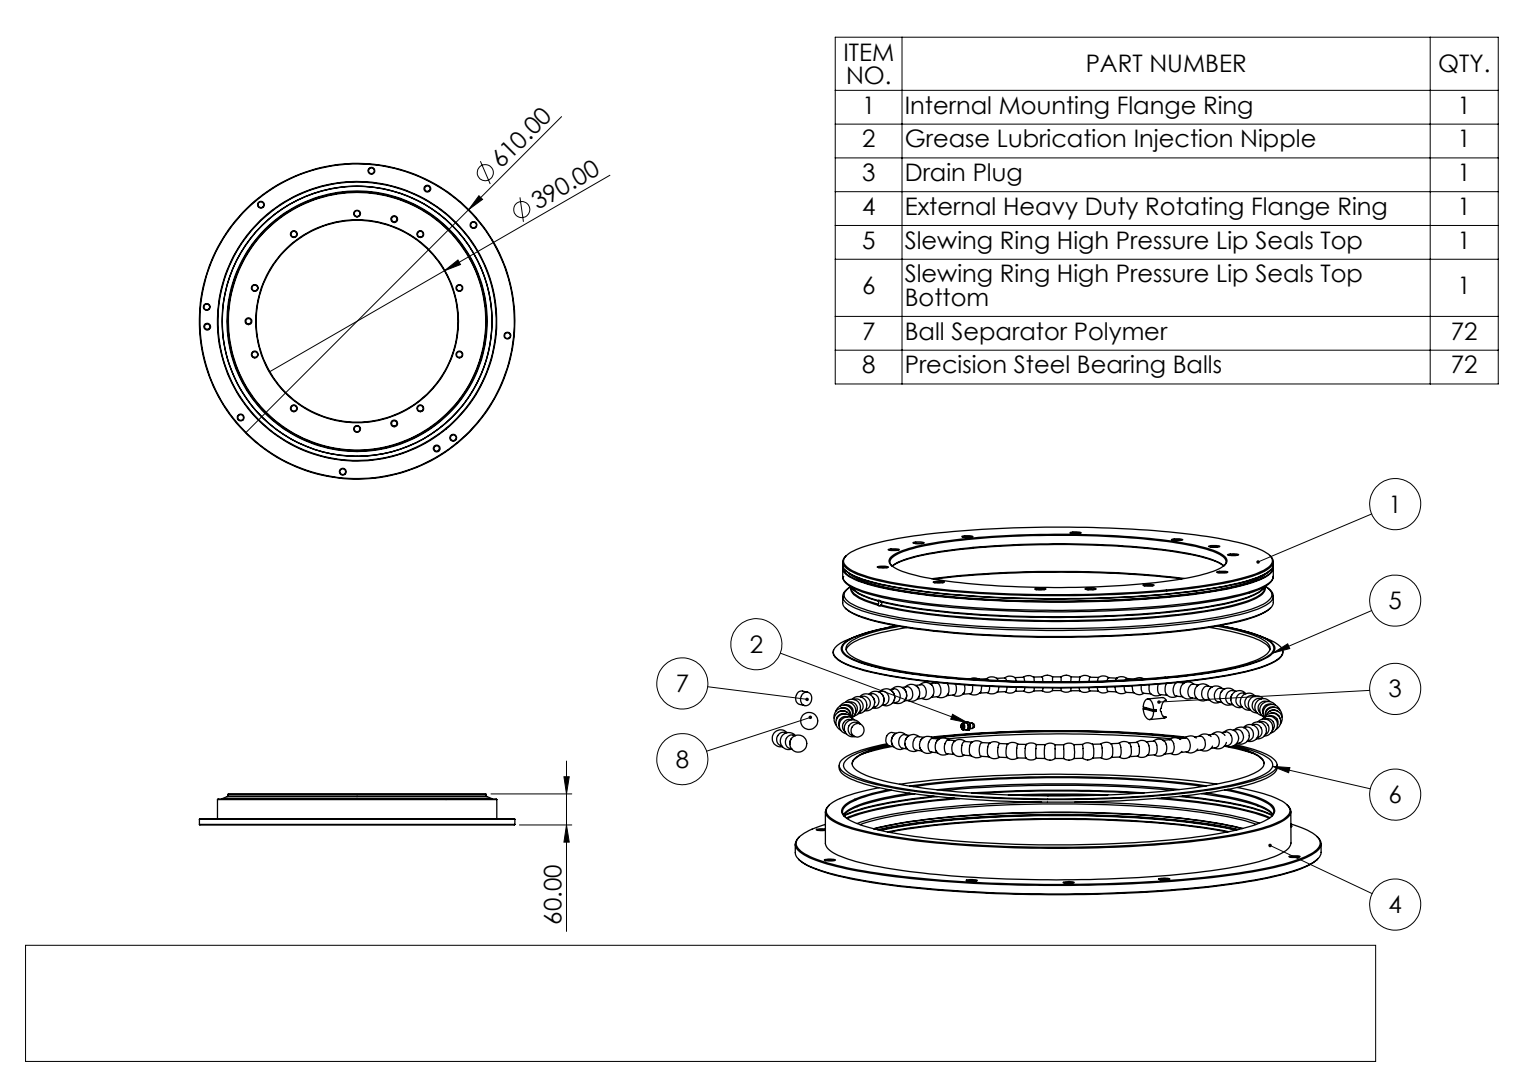
ISO-10303-21;
HEADER;
FILE_DESCRIPTION (('STEP AP214'),
    '1' );
FILE_NAME ('MAS-489',
    '2026-10-09T12:49:55',
    ( '' ),
    ( '' ),
    'SwSTEP 2.0',
    'SolidWorks 2026',
    '' );
FILE_SCHEMA (( 'AUTOMOTIVE_DESIGN' ));
ENDSEC;

DATA;
#1 = CARTESIAN_POINT ( 'NONE',  ( -244.7604950974910878, 8.603785962528602838, 8.365103762022689793 ) ) ;
#2 = VECTOR ( 'NONE', #2010, 1000.000000000000000 ) ;
#3 = DIRECTION ( 'NONE',  ( 0.6378047977532573798, 0.5538822189107470706, -0.5351817705578485462 ) ) ;
#4 = CARTESIAN_POINT ( 'NONE',  ( 227.3999999999999773, -2.172755033604258923, 3.940702420120982374 ) ) ;
#5 = TOROIDAL_SURFACE ( 'NONE', #5776, 250.0000000000000000, 10.00000000000000000 ) ;
#6 = ITEM_DEFINED_TRANSFORMATION ( 'NONE', 'NONE', #11295,  #805 ) ;
#7 = CARTESIAN_POINT ( 'NONE',  ( 222.8706404512946904, 0.000000000000000000, 0.000000000000000000 ) ) ;
#8 = EDGE_LOOP ( 'NONE', ( #2627, #6093, #4363, #303 ) ) ;
#9 = ORIENTED_EDGE ( 'NONE', *, *, #8914, .T. ) ;
#10 = CONICAL_SURFACE ( 'NONE', #3613, 1.750000000000000000, 0.4188790204786330129 ) ;
#11 = CARTESIAN_POINT ( 'NONE',  ( -34.18476129408180242, 19.96883745937779864, 259.4723857443443080 ) ) ;
#12 = DIRECTION ( 'NONE',  ( 0.000000000000000000, -1.000000000000000000, 0.000000000000000000 ) ) ;
#13 = ADVANCED_FACE ( 'NONE', ( #7160 ), #9859, .F. ) ;
#14 = EDGE_CURVE ( 'NONE', #2438, #5570, #3411, .T. ) ;
#15 = DIRECTION ( 'NONE',  ( 0.6368676505102708330, 0.000000000000000000, 0.7709731485165535192 ) ) ;
#16 = AXIS2_PLACEMENT_3D ( 'NONE', #743, #4857, #3859 ) ;
#17 = CARTESIAN_POINT ( 'NONE',  ( 17.06760680892275062, 20.79694577654979071, 260.7745447056980197 ) ) ;
#18 = CYLINDRICAL_SURFACE ( 'NONE', #6462, 5.500000000000005329 ) ;
#19 = DIRECTION ( 'NONE',  ( 0.5735764363510555963, 0.000000000000000000, -0.8191520442889851372 ) ) ;
#20 = CARTESIAN_POINT ( 'NONE',  ( -243.1949234122827193, -7.480730365350286348, 9.061063672199042074 ) ) ;
#21 = CONTEXT_DEPENDENT_SHAPE_REPRESENTATION ( #3190, #1979 ) ;
#22 = ORIENTED_EDGE ( 'NONE', *, *, #3438, .F. ) ;
#23 = CARTESIAN_POINT ( 'NONE',  ( -230.0000000000000000, 18.00000000000000000, 0.000000000000000000 ) ) ;
#24 = LINE ( 'NONE', #4986, #10827 ) ;
#25 = CARTESIAN_POINT ( 'NONE',  ( 0.000000000000000000, 22.00000000000000000, 0.000000000000000000 ) ) ;
#26 = EDGE_LOOP ( 'NONE', ( #5879, #12768 ) ) ;
#27 = ORIENTED_EDGE ( 'NONE', *, *, #7436, .F. ) ;
#28 = DIRECTION ( 'NONE',  ( 0.000000000000000000, 1.000000000000000000, 0.000000000000000000 ) ) ;
#29 = PLANE ( 'NONE',  #10608 ) ;
#30 = CARTESIAN_POINT ( 'NONE',  ( -247.8175805190998062, 19.96883746075563693, 84.14846197946620521 ) ) ;
#31 = VECTOR ( 'NONE', #3967, 1000.000000000000000 ) ;
#32 = STYLED_ITEM ( 'NONE', ( #1106 ), #1548 ) ;
#33 = CARTESIAN_POINT ( 'NONE',  ( 122.2593324768346008, 18.00000000000000000, 161.7755348299889988 ) ) ;
#34 = AXIS2_PLACEMENT_3D ( 'NONE', #11717, #7639, #3504 ) ;
#35 = DIRECTION ( 'NONE',  ( 0.9659258262890680902, 0.000000000000000000, 0.2588190451025213501 ) ) ;
#36 = CARTESIAN_POINT ( 'NONE',  ( -244.7823818444411188, 8.610125652527095497, 7.996289171610727387 ) ) ;
#37 = EDGE_LOOP ( 'NONE', ( #12294, #12083 ) ) ;
#38 = CARTESIAN_POINT ( 'NONE',  ( 206.9952515782970295, 20.79694577634646535, 158.8368823490022237 ) ) ;
#39 = EDGE_CURVE ( 'NONE', #10768, #6987, #12629, .T. ) ;
#41 = ORIENTED_EDGE ( 'NONE', *, *, #3287, .F. ) ;
#40 = AXIS2_PLACEMENT_3D ( 'NONE', #6246, #10297, #1175 ) ;
#42 = EDGE_CURVE ( 'NONE', #9318, #6702, #6889, .T. ) ;
#43 = CARTESIAN_POINT ( 'NONE',  ( 6.735557395310442023E-16, 19.00000000000000000, 213.5000000000000000 ) ) ;
#44 = ORIENTED_EDGE ( 'NONE', *, *, #3957, .F. ) ;
#45 = CARTESIAN_POINT ( 'NONE',  ( -248.8440518482232733, 9.943161799075943108, -6.718187330775476696 ) ) ;
#46 =( REPRESENTATION_RELATIONSHIP ('NONE','NONE', #12019, #182 ) REPRESENTATION_RELATIONSHIP_WITH_TRANSFORMATION ( #319 )SHAPE_REPRESENTATION_RELATIONSHIP( ) );
#47 = DIRECTION ( 'NONE',  ( -0.000000000000000000, 1.000000000000000000, 0.000000000000000000 ) ) ;
#48 = SURFACE_SIDE_STYLE ('',( #1037 ) ) ;
#49 = CYLINDRICAL_SURFACE ( 'NONE', #12751, 249.7999999999999829 ) ;
#50 = CARTESIAN_POINT ( 'NONE',  ( 6.735557395310442023E-16, 19.00000000000000000, -202.4999999999999716 ) ) ;
#51 = CARTESIAN_POINT ( 'NONE',  ( 6.345753394971347358E-13, 20.08915143297736350, -260.5542428351130866 ) ) ;
#52 = DIRECTION ( 'NONE',  ( 0.000000000000000000, -1.000000000000000000, 0.000000000000000000 ) ) ;
#53 = CARTESIAN_POINT ( 'NONE',  ( -137.7829567244536122, 20.79694577634646890, 221.5672498511017920 ) ) ;
#54 = ITEM_DEFINED_TRANSFORMATION ( 'NONE', 'NONE', #1459,  #805 ) ;
#55 = ORIENTED_EDGE ( 'NONE', *, *, #3049, .F. ) ;
#56 = CARTESIAN_POINT ( 'NONE',  ( 220.3999999999999773, 2.249562960690858038, -0.04434507737934524629 ) ) ;
#57 = CIRCLE ( 'NONE', #1754, 6.500000000000005329 ) ;
#58 = VERTEX_POINT ( 'NONE', #5076 ) ;
#59 = EDGE_CURVE ( 'NONE', #2857, #11921, #819, .T. ) ;
#60 = CIRCLE ( 'NONE', #11338, 5.499999999999986677 ) ;
#61 = CARTESIAN_POINT ( 'NONE',  ( -249.1369139485392168, 10.36343465138863529, -5.538914405136962316 ) ) ;
#62 = CARTESIAN_POINT ( 'NONE',  ( -246.4289107134841004, -9.384359667671809291, -7.479355995036127247 ) ) ;
#63 =( REPRESENTATION_RELATIONSHIP ('NONE','NONE', #12019, #182 ) REPRESENTATION_RELATIONSHIP_WITH_TRANSFORMATION ( #9414 )SHAPE_REPRESENTATION_RELATIONSHIP( ) );
#64 = DIRECTION ( 'NONE',  ( 0.6368676505102698338, 0.000000000000000000, 0.7709731485165541853 ) ) ;
#65 = ORIENTED_EDGE ( 'NONE', *, *, #5983, .T. ) ;
#66 = ADVANCED_FACE ( 'NONE', ( #7091 ), #10088, .F. ) ;
#67 = CARTESIAN_POINT ( 'NONE',  ( 84.02568524182660781, 20.79694577630801078, -247.4557548099990072 ) ) ;
#68 = DIRECTION ( 'NONE',  ( 8.659560562354926695E-17, 0.7071067811865480168, -0.7071067811865470176 ) ) ;
#69 = CARTESIAN_POINT ( 'NONE',  ( -239.9450917581429792, -2.156506209390995021, 11.80463811257499884 ) ) ;
#70 = AXIS2_PLACEMENT_3D ( 'NONE', #7490, #8365, #9292 ) ;
#71 = CARTESIAN_POINT ( 'NONE',  ( -245.4148443366356389, -8.946846751066603431, -7.616852152915439156 ) ) ;
#72 = DIRECTION ( 'NONE',  ( 0.7545873610930060593, 0.5538822189107471816, -0.3518698652246315395 ) ) ;
#73 = CARTESIAN_POINT ( 'NONE',  ( -229.7583704989254443, -5.204493534573133573, 10.54155285988093382 ) ) ;
#74 = PRODUCT_DEFINITION_SHAPE ( 'NONE', 'NONE',  #13116 ) ;
#75 = CIRCLE ( 'NONE', #5391, 251.1999999999999886 ) ;
#76 = CARTESIAN_POINT ( 'NONE',  ( 0.000000000000000000, -23.50000000000000000, 0.000000000000000000 ) ) ;
#77 = AXIS2_PLACEMENT_3D ( 'NONE', #6499, #10557, #9543 ) ;
#78 = ORIENTED_EDGE ( 'NONE', *, *, #7931, .F. ) ;
#79 = ORIENTED_EDGE ( 'NONE', *, *, #10538, .F. ) ;
#80 = CARTESIAN_POINT ( 'NONE',  ( 247.2466869557899827, 20.08915143289970473, -83.95474316006121285 ) ) ;
#81 = CARTESIAN_POINT ( 'NONE',  ( 11.00000000000000000, 0.000000000000000000, 259.9000000000000341 ) ) ;
#82 = FACE_OUTER_BOUND ( 'NONE', #8092, .T. ) ;
#83 = DIRECTION ( 'NONE',  ( -0.000000000000000000, -1.000000000000000000, 0.000000000000000000 ) ) ;
#84 = CIRCLE ( 'NONE', #11996, 6.500000000000005329 ) ;
#85 = CARTESIAN_POINT ( 'NONE',  ( -1.010328782420808020E-12, 20.79694577634649022, 260.7745447061710138 ) ) ;
#86 = CARTESIAN_POINT ( 'NONE',  ( -182.4625818711933221, -29.00000000000000000, -220.8838070499919297 ) ) ;
#87 = DIRECTION ( 'NONE',  ( 0.9659258262890654256, 0.000000000000000000, 0.2588190451025314531 ) ) ;
#88 = CONICAL_SURFACE ( 'NONE', #12605, 5.500000000000005329, 0.7853981633974461696 ) ;
#89 = CARTESIAN_POINT ( 'NONE',  ( -243.1551830321760690, -7.446108171798711872, 9.089443071778552152 ) ) ;
#90 = VERTEX_POINT ( 'NONE', #9222 ) ;
#91 = FACE_BOUND ( 'NONE', #3077, .T. ) ;
#92 = EDGE_CURVE ( 'NONE', #10082, #1949, #2942, .T. ) ;
#93 = DIRECTION ( 'NONE',  ( 0.000000000000000000, 1.000000000000000000, 0.000000000000000000 ) ) ;
#94 = ORIENTED_EDGE ( 'NONE', *, *, #12232, .T. ) ;
#95 = ORIENTED_EDGE ( 'NONE', *, *, #11589, .F. ) ;
#96 = CONICAL_SURFACE ( 'NONE', #12225, 250.1999999999999602, 0.7853981633975041232 ) ;
#97 = DIRECTION ( 'NONE',  ( 0.000000000000000000, 0.000000000000000000, -1.000000000000000000 ) ) ;
#98 = FACE_BOUND ( 'NONE', #10727, .T. ) ;
#99 = CARTESIAN_POINT ( 'NONE',  ( 34.18476129334108293, 19.96883746037050855, -259.4723857425807978 ) ) ;
#100 = CARTESIAN_POINT ( 'NONE',  ( -294.8238222686197787, -18.00000000000000000, -32.70078231947154279 ) ) ;
#101 = CARTESIAN_POINT ( 'NONE',  ( 0.000000000000000000, 0.000000000000000000, 0.000000000000000000 ) ) ;
#102 = CARTESIAN_POINT ( 'NONE',  ( -243.6022064859786269, 7.815160994106106429, 8.774769236968495534 ) ) ;
#103 = CONICAL_SURFACE ( 'NONE', #1806, 5.500000000000005329, 0.7853981633974461696 ) ;
#104 = AXIS2_PLACEMENT_3D ( 'NONE', #9793, #603, #2593 ) ;
#105 = EDGE_LOOP ( 'NONE', ( #5377, #568, #8957, #6732 ) ) ;
#106 = FACE_OUTER_BOUND ( 'NONE', #3222, .T. ) ;
#107 = EDGE_CURVE ( 'NONE', #6490, #4415, #2518, .T. ) ;
#108 = EDGE_LOOP ( 'NONE', ( #11966, #7349 ) ) ;
#109 = CARTESIAN_POINT ( 'NONE',  ( 234.3487510399341716, 2.474519256759935448, -0.04877958511727960994 ) ) ;
#110 = ORIENTED_EDGE ( 'NONE', *, *, #7597, .T. ) ;
#111 = ORIENTED_EDGE ( 'NONE', *, *, #3767, .F. ) ;
#112 = CIRCLE ( 'NONE', #2851, 5.500000000000007994 ) ;
#113 = CARTESIAN_POINT ( 'NONE',  ( 229.2637990951503753, -30.00000000000000000, -180.9540284836414514 ) ) ;
#114 = FILL_AREA_STYLE_COLOUR ( '', #3598 ) ;
#115 = PRODUCT ( 'MAS-489', 'MAS-489', '', ( #1262 ) ) ;
#116 = CARTESIAN_POINT ( 'NONE',  ( 239.1963018252363042, 1.024882057239583366, 3.346595946712579206 ) ) ;
#117 = EDGE_CURVE ( 'NONE', #171, #5643, #5501, .T. ) ;
#118 = DIRECTION ( 'NONE',  ( -0.000000000000000000, -1.000000000000000000, 0.000000000000000000 ) ) ;
#119 = EDGE_CURVE ( 'NONE', #4577, #1020, #8907, .T. ) ;
#120 = CARTESIAN_POINT ( 'NONE',  ( -238.7109915777814138, -2.671037648644427152E-08, -11.74999999995326050 ) ) ;
#121 = DIRECTION ( 'NONE',  ( 0.000000000000000000, 1.000000000000000000, 0.000000000000000000 ) ) ;
#122 = ITEM_DEFINED_TRANSFORMATION ( 'NONE', 'NONE', #4000,  #805 ) ;
#123 = ORIENTED_EDGE ( 'NONE', *, *, #7186, .T. ) ;
#124 = DIRECTION ( 'NONE',  ( -0.6368676505102700558, 0.000000000000000000, -0.7709731485165541853 ) ) ;
#125 = AXIS2_PLACEMENT_3D ( 'NONE', #10456, #7067, #12062 ) ;
#126 = ORIENTED_EDGE ( 'NONE', *, *, #7506, .T. ) ;
#127 = CIRCLE ( 'NONE', #974, 239.8169934640564804 ) ;
#128 = FACE_OUTER_BOUND ( 'NONE', #4868, .T. ) ;
#129 = CARTESIAN_POINT ( 'NONE',  ( -248.5349130519067558, -9.924317173753149035, -6.749248572539269020 ) ) ;
#130 = CARTESIAN_POINT ( 'NONE',  ( 67.47543992452018813, 20.08915143297736705, -251.8100110699623713 ) ) ;
#131 = EDGE_LOOP ( 'NONE', ( #6897, #5787, #9258, #12917 ) ) ;
#132 = CARTESIAN_POINT ( 'NONE',  ( 252.4341100445949735, 20.79694577582237613, 67.61424742981928659 ) ) ;
#133 = CARTESIAN_POINT ( 'NONE',  ( -244.3545189613893172, 8.356296381722604139, -8.612604416346371750 ) ) ;
#134 = DIRECTION ( 'NONE',  ( 0.000000000000000000, 0.000000000000000000, 1.000000000000000000 ) ) ;
#135 = EDGE_CURVE ( 'NONE', #12433, #12610, #12359, .T. ) ;
#136 = CARTESIAN_POINT ( 'NONE',  ( -243.1925160140377216, -7.478514340598183097, -9.062807757124144103 ) ) ;
#137 = ADVANCED_FACE ( 'NONE', ( #98, #7027 ), #29, .F. ) ;
#138 = CARTESIAN_POINT ( 'NONE',  ( 39.32730324096118579, -138.4705547276867321, 14.31396777367110928 ) ) ;
#139 = CARTESIAN_POINT ( 'NONE',  ( 240.4181131690920097, 2.891045149275324633, 1.982248008065000233 ) ) ;
#140 = EDGE_CURVE ( 'NONE', #10237, #12935, #11247, .T. ) ;
#141 = ITEM_DEFINED_TRANSFORMATION ( 'NONE', 'NONE', #2560,  #805 ) ;
#142 = CARTESIAN_POINT ( 'NONE',  ( -27.68945685411286561, -30.00000000000000000, 290.6841825403027997 ) ) ;
#143 = ORIENTED_EDGE ( 'NONE', *, *, #1183, .T. ) ;
#144 = ORIENTED_EDGE ( 'NONE', *, *, #3305, .F. ) ;
#145 = CARTESIAN_POINT ( 'NONE',  ( -172.1812796679919870, 20.08915143287683591, 196.2980642839890209 ) ) ;
#146 = FACE_OUTER_BOUND ( 'NONE', #6350, .T. ) ;
#147 = CARTESIAN_POINT ( 'NONE',  ( 239.5387464286556565, -1.581210110862248941, -3.124650852508605858 ) ) ;
#148 = CARTESIAN_POINT ( 'NONE',  ( -185.9653539489998195, -30.00000000000000000, -225.1241593668329699 ) ) ;
#149 = DIRECTION ( 'NONE',  ( 0.000000000000000000, 1.000000000000000000, 0.000000000000000000 ) ) ;
#150 = CARTESIAN_POINT ( 'NONE',  ( 0.000000000000000000, -9.830508068699650437, 0.000000000000000000 ) ) ;
#151 = DIRECTION ( 'NONE',  ( 0.3420201433256790380, 0.000000000000000000, -0.9396926207859046531 ) ) ;
#152 = CARTESIAN_POINT ( 'NONE',  ( -246.6649006625763718, -9.461692665201230312, 6.966985664009688328 ) ) ;
#153 =( REPRESENTATION_RELATIONSHIP ('NONE','NONE', #12019, #5191 ) REPRESENTATION_RELATIONSHIP_WITH_TRANSFORMATION ( #11550 )SHAPE_REPRESENTATION_RELATIONSHIP( ) );
#154 = EDGE_LOOP ( 'NONE', ( #1351, #3008, #4241, #9314 ) ) ;
#155 = CARTESIAN_POINT ( 'NONE',  ( 240.6084075703383292, -3.437342788167941698, 0.6677429272691086659 ) ) ;
#156 = CARTESIAN_POINT ( 'NONE',  ( 229.9948761773756587, -3.146545554286515056, -1.549783278019676303 ) ) ;
#157 = VERTEX_POINT ( 'NONE', #8121 ) ;
#158 = VERTEX_POINT ( 'NONE', #1956 ) ;
#159 = CARTESIAN_POINT ( 'NONE',  ( 122.2593324768334071, 18.00000000000000000, -168.2755348299895104 ) ) ;
#160 = DIRECTION ( 'NONE',  ( 0.000000000000000000, 1.000000000000000000, 0.000000000000000000 ) ) ;
#161 = EDGE_CURVE ( 'NONE', #12208, #12419, #5216, .T. ) ;
#162 = CARTESIAN_POINT ( 'NONE',  ( -172.5787240293117293, 19.96883745935916821, -196.7513681803530403 ) ) ;
#163 = AXIS2_PLACEMENT_3D ( 'NONE', #4831, #2895, #11790 ) ;
#164 = LINE ( 'NONE', #1161, #5159 ) ;
#165 = SHAPE_REPRESENTATION_RELATIONSHIP ( 'NONE' , 'NONE' ,  #182, #11264 ) ;
#166 = CARTESIAN_POINT ( 'NONE',  ( -242.4885533041308179, 6.811171349317773682, 9.574815119040657407 ) ) ;
#167 = VERTEX_POINT ( 'NONE', #4213 ) ;
#168 = CARTESIAN_POINT ( 'NONE',  ( 158.8368823490023374, 20.79694577634646535, 206.9952515782968874 ) ) ;
#169 = VERTEX_POINT ( 'NONE', #4404 ) ;
#170 = CARTESIAN_POINT ( 'NONE',  ( 226.1499999999999773, 0.000000000000000000, 0.000000000000000000 ) ) ;
#171 = VERTEX_POINT ( 'NONE', #8621 ) ;
#172 = ORIENTED_EDGE ( 'NONE', *, *, #9218, .F. ) ;
#173 =( REPRESENTATION_RELATIONSHIP ('NONE','NONE', #12019, #5191 ) REPRESENTATION_RELATIONSHIP_WITH_TRANSFORMATION ( #7916 )SHAPE_REPRESENTATION_RELATIONSHIP( ) );
#174 = DIRECTION ( 'NONE',  ( 0.000000000000000000, -1.000000000000000000, 0.000000000000000000 ) ) ;
#175 = FACE_OUTER_BOUND ( 'NONE', #11352, .T. ) ;
#176 = ADVANCED_FACE ( 'NONE', ( #6424 ), #11036, .F. ) ;
#177 = ADVANCED_FACE ( 'NONE', ( #3475, #8488, #10550, #7486, #12547, #4470, #3403, #10415, #12679, #11557, #2351, #9424, #1290 ), #8427, .F. ) ;
#178 = DIRECTION ( 'NONE',  ( 0.000000000000000000, 0.000000000000000000, 1.000000000000000000 ) ) ;
#179 = CARTESIAN_POINT ( 'NONE',  ( -206.8203823583188807, 20.08915143297736705, -158.7026972336036295 ) ) ;
#180 = LINE ( 'NONE', #8188, #691 ) ;
#181 = AXIS2_PLACEMENT_3D ( 'NONE', #12668, #7601, #11676 ) ;
#182 = SHAPE_REPRESENTATION ( 'Precision Steel Bearing Balls', ( #805 ), #1451 ) ;
#183 = ORIENTED_EDGE ( 'NONE', *, *, #8273, .T. ) ;
#184 = EDGE_LOOP ( 'NONE', ( #4999, #5010, #6703, #1968 ) ) ;
#185 = DIRECTION ( 'NONE',  ( 0.000000000000000000, 0.000000000000000000, 1.000000000000000000 ) ) ;
#186 = DIRECTION ( 'NONE',  ( 0.000000000000000000, 1.000000000000000000, 0.000000000000000000 ) ) ;
#187 = DIRECTION ( 'NONE',  ( 0.6368676505102709440, 0.000000000000000000, 0.7709731485165532971 ) ) ;
#188 = CIRCLE ( 'NONE', #5900, 6.499999999999999112 ) ;
#189 = EDGE_LOOP ( 'NONE', ( #9728, #4932, #9679, #1428 ) ) ;
#190 = VECTOR ( 'NONE', #5245, 1000.000000000000000 ) ;
#191 = CIRCLE ( 'NONE', #10174, 8.000000000000007105 ) ;
#192 = AXIS2_PLACEMENT_3D ( 'NONE', #6124, #12263, #134 ) ;
#193 = CARTESIAN_POINT ( 'NONE',  ( 252.4341100441809829, 20.79694577595645910, -67.61424743030308093 ) ) ;
#194 = CARTESIAN_POINT ( 'NONE',  ( -244.9313462844523315, 8.700834631118880225, -8.264179333829037688 ) ) ;
#195 = CARTESIAN_POINT ( 'NONE',  ( -159.9811538081800393, -30.00000000000000000, -193.6684549073582389 ) ) ;
#196 = CARTESIAN_POINT ( 'NONE',  ( -246.9758887735252699, -9.561393943077655777, -6.829510937495726353 ) ) ;
#197 = CIRCLE ( 'NONE', #11695, 196.0000000000000000 ) ;
#198 = DIRECTION ( 'NONE',  ( 0.7071067811865561215, 0.000000000000000000, -0.7071067811865389130 ) ) ;
#199 = CARTESIAN_POINT ( 'NONE',  ( 240.6075165363340318, 3.437532598196324063, 0.7648284528981581509 ) ) ;
#200 = EDGE_CURVE ( 'NONE', #7619, #9887, #12317, .T. ) ;
#201 = EDGE_CURVE ( 'NONE', #6448, #6354, #188, .T. ) ;
#202 = CARTESIAN_POINT ( 'NONE',  ( 84.02568524192950861, 20.79694577611522632, 247.4557548104415048 ) ) ;
#203 = CIRCLE ( 'NONE', #9142, 2.000000000000001776 ) ;
#204 = VERTEX_POINT ( 'NONE', #489 ) ;
#205 = CARTESIAN_POINT ( 'NONE',  ( 258.8746690706130380, 20.08915143329827657, -34.10614053547809732 ) ) ;
#206 = DIRECTION ( 'NONE',  ( 0.6368676505102707219, 0.000000000000000000, 0.7709731485165535192 ) ) ;
#207 = CARTESIAN_POINT ( 'NONE',  ( -248.9051445890450225, 10.17462340872661741, 5.878044170807267044 ) ) ;
#208 = DIRECTION ( 'NONE',  ( 0.000000000000000000, 0.7071067811865480168, 0.7071067811865470176 ) ) ;
#209 = DIRECTION ( 'NONE',  ( 8.659560562354913137E-17, -0.7071067811865489050, 0.7071067811865460184 ) ) ;
#210 = CARTESIAN_POINT ( 'NONE',  ( -249.3376476200290028, -9.985526825745921542, 6.655116011123642927 ) ) ;
#211 = DIRECTION ( 'NONE',  ( 0.000000000000000000, 0.000000000000000000, 1.000000000000000000 ) ) ;
#212 = DIRECTION ( 'NONE',  ( 0.9848077530122105738, 0.000000000000000000, -0.1736481776669172861 ) ) ;
#213 = DIRECTION ( 'NONE',  ( 0.000000000000000000, 0.000000000000000000, -1.000000000000000000 ) ) ;
#214 = CONTEXT_DEPENDENT_SHAPE_REPRESENTATION ( #9747, #1764 ) ;
#215 = ORIENTED_EDGE ( 'NONE', *, *, #11212, .T. ) ;
#216 = DIRECTION ( 'NONE',  ( 0.000000000000000000, 0.000000000000000000, 1.000000000000000000 ) ) ;
#217 = AXIS2_PLACEMENT_3D ( 'NONE', #2589, #10592, #3388 ) ;
#218 = EDGE_CURVE ( 'NONE', #9833, #1462, #5421, .T. ) ;
#219 = PRODUCT ( 'Grease Lubrication Injection Nipple', 'Grease Lubrication Injection Nipple', '', ( #6400 ) ) ;
#220 = CYLINDRICAL_SURFACE ( 'NONE', #828, 246.0000000000000000 ) ;
#221 = ORIENTED_EDGE ( 'NONE', *, *, #12738, .T. ) ;
#222 = ORIENTED_EDGE ( 'NONE', *, *, #3793, .T. ) ;
#223 = FACE_OUTER_BOUND ( 'NONE', #154, .T. ) ;
#224 = DIRECTION ( 'NONE',  ( 0.000000000000000000, 0.000000000000000000, 1.000000000000000000 ) ) ;
#225 = CARTESIAN_POINT ( 'NONE',  ( -252.9796497735838443, 20.55460285104794949, 67.76049180365761515 ) ) ;
#226 = LINE ( 'NONE', #5219, #2394 ) ;
#227 = CARTESIAN_POINT ( 'NONE',  ( 0.000000000000000000, 0.000000000000000000, 0.000000000000000000 ) ) ;
#228 = DIRECTION ( 'NONE',  ( 0.000000000000000000, 0.000000000000000000, 1.000000000000000000 ) ) ;
#229 = AXIS2_PLACEMENT_3D ( 'NONE', #9662, #409, #545 ) ;
#230 = ORIENTED_EDGE ( 'NONE', *, *, #4416, .F. ) ;
#231 = DIRECTION ( 'NONE',  ( 1.000000000000000000, 0.000000000000000000, 0.000000000000000000 ) ) ;
#232 = ORIENTED_EDGE ( 'NONE', *, *, #7024, .T. ) ;
#233 = CARTESIAN_POINT ( 'NONE',  ( 135.8846079354933352, -18.00000000000000000, -256.1940150085812888 ) ) ;
#234 = ORIENTED_EDGE ( 'NONE', *, *, #10382, .T. ) ;
#235 = ORIENTED_EDGE ( 'NONE', *, *, #8600, .T. ) ;
#236 = CARTESIAN_POINT ( 'NONE',  ( 222.0845275804282153, 0.000000000000000000, 0.000000000000000000 ) ) ;
#237 = VERTEX_POINT ( 'NONE', #3498 ) ;
#238 = DIRECTION ( 'NONE',  ( 0.000000000000000000, 1.000000000000000000, 0.000000000000000000 ) ) ;
#239 = CARTESIAN_POINT ( 'NONE',  ( -171.9542656377731475, 19.00000000000000000, -208.1627500994694344 ) ) ;
#240 = CARTESIAN_POINT ( 'NONE',  ( 11.00000000000000000, 0.000000000000000000, 250.0000000000000000 ) ) ;
#241 = CARTESIAN_POINT ( 'NONE',  ( -233.0000000000000000, 1.000000000000000000, 11.95826074310140008 ) ) ;
#242 = CARTESIAN_POINT ( 'NONE',  ( -243.4813404522815574, 7.728679802368522367, 9.179736092244874968 ) ) ;
#243 = DIRECTION ( 'NONE',  ( 0.000000000000000000, -0.7071067811865489050, -0.7071067811865460184 ) ) ;
#244 = CONTEXT_DEPENDENT_SHAPE_REPRESENTATION ( #46, #6907 ) ;
#245 = ORIENTED_EDGE ( 'NONE', *, *, #2691, .F. ) ;
#246 = DIRECTION ( 'NONE',  ( 0.9135454576426030870, 0.4066576386751317163, -0.008016341293427224970 ) ) ;
#247 = AXIS2_PLACEMENT_3D ( 'NONE', #6656, #10577, #2507 ) ;
#248 = CARTESIAN_POINT ( 'NONE',  ( -249.2724874750463755, -10.50618518648515476, 5.261424415983393388 ) ) ;
#249 = ORIENTED_EDGE ( 'NONE', *, *, #11663, .F. ) ;
#250 = DIRECTION ( 'NONE',  ( -0.6368676505102706109, 0.000000000000000000, -0.7709731485165535192 ) ) ;
#251 = DIRECTION ( 'NONE',  ( -0.000000000000000000, -1.000000000000000000, 0.000000000000000000 ) ) ;
#252 = EDGE_CURVE ( 'NONE', #8118, #6913, #791, .T. ) ;
#253 = EDGE_CURVE ( 'NONE', #823, #11992, #3550, .T. ) ;
#254 = DIRECTION ( 'NONE',  ( 0.000000000000000000, 0.000000000000000000, 1.000000000000000000 ) ) ;
#255 = ORIENTED_EDGE ( 'NONE', *, *, #1182, .T. ) ;
#256 = CARTESIAN_POINT ( 'NONE',  ( -233.0000000000000000, 0.000000000000000000, 0.000000000000000000 ) ) ;
#257 = CARTESIAN_POINT ( 'NONE',  ( -241.6004288480548610, 5.767183905335713234, -10.52387470031727368 ) ) ;
#258 = CARTESIAN_POINT ( 'NONE',  ( -238.7266973618091299, 0.3758472202226714187, 11.99420542475303009 ) ) ;
#259 = CARTESIAN_POINT ( 'NONE',  ( -229.9627996858143888, 10.99879348686639879, 4.151745503392231029 ) ) ;
#260 = AXIS2_PLACEMENT_3D ( 'NONE', #6805, #2654, #10860 ) ;
#261 = FILL_AREA_STYLE_COLOUR ( '', #9272 ) ;
#262 = APPLICATION_PROTOCOL_DEFINITION ( 'draft international standard', 'automotive_design', 1998, #8164 ) ;
#263 = CARTESIAN_POINT ( 'NONE',  ( -229.6996873213522008, 2.466058644897756835, -11.74980236389214028 ) ) ;
#264 = CONTEXT_DEPENDENT_SHAPE_REPRESENTATION ( #5876, #9605 ) ;
#265 = AXIS2_PLACEMENT_3D ( 'NONE', #9269, #11198, #3992 ) ;
#266 = FACE_OUTER_BOUND ( 'NONE', #2939, .T. ) ;
#267 = ORIENTED_EDGE ( 'NONE', *, *, #6171, .T. ) ;
#268 = CONICAL_SURFACE ( 'NONE', #4306, 251.1999999999999886, 0.7853981633974207455 ) ;
#269 = CARTESIAN_POINT ( 'NONE',  ( 172.1812796672219861, 20.08915143311016749, 196.2980642831085163 ) ) ;
#270 = PLANE ( 'NONE',  #8814 ) ;
#271 = CARTESIAN_POINT ( 'NONE',  ( -233.0000000000000000, -1.000000000000000000, -11.95826074310140008 ) ) ;
#272 = CONICAL_SURFACE ( 'NONE', #12608, 6.500000000000005329, 0.7853981633974617127 ) ;
#273 = CARTESIAN_POINT ( 'NONE',  ( -249.2624683435426789, 10.49496574114239422, 5.283769351005206616 ) ) ;
#274 = CARTESIAN_POINT ( 'NONE',  ( 122.2593324768334071, 30.00000000000000000, -161.7755348299894820 ) ) ;
#275 = CARTESIAN_POINT ( 'NONE',  ( 3.077430737863366313E-14, 21.94174202707280941, -251.2912898646363828 ) ) ;
#276 = ADVANCED_FACE ( 'NONE', ( #8553 ), #7175, .F. ) ;
#277 = CARTESIAN_POINT ( 'NONE',  ( -247.9991062040697045, -9.816924796812509513, 6.901310522868776332 ) ) ;
#278 = EDGE_CURVE ( 'NONE', #2702, #9134, #8362, .T. ) ;
#279 = CARTESIAN_POINT ( 'NONE',  ( -159.2169126275676945, -3.061616997868385015E-14, -192.7432871291383663 ) ) ;
#280 = DIRECTION ( 'NONE',  ( -0.2847642722309865482, 0.5538822189107472926, 0.7823834078220627264 ) ) ;
#281 = AXIS2_PLACEMENT_3D ( 'NONE', #8351, #12412, #4459 ) ;
#282 = CARTESIAN_POINT ( 'NONE',  ( 161.8917567597108018, -25.00000000000000000, 195.9813743529078920 ) ) ;
#283 = CONTEXT_DEPENDENT_SHAPE_REPRESENTATION ( #63, #74 ) ;
#284 = EDGE_LOOP ( 'NONE', ( #11200, #1188, #5610, #7256 ) ) ;
#285 = AXIS2_PLACEMENT_3D ( 'NONE', #10507, #6446, #1378 ) ;
#286 = CARTESIAN_POINT ( 'NONE',  ( -249.7118339206215012, -9.997999799959989886, 6.636264009214830395 ) ) ;
#287 = CARTESIAN_POINT ( 'NONE',  ( 0.000000000000000000, 2.772967769359004908, 0.000000000000000000 ) ) ;
#288 = EDGE_LOOP ( 'NONE', ( #12624, #10639, #6520, #4840 ) ) ;
#289 = ORIENTED_EDGE ( 'NONE', *, *, #5424, .F. ) ;
#290 = CARTESIAN_POINT ( 'NONE',  ( 0.000000000000000000, 2.772967769358929857, 0.000000000000000000 ) ) ;
#291 = DIRECTION ( 'NONE',  ( -0.000000000000000000, -1.000000000000000000, 0.000000000000000000 ) ) ;
#292 = PRODUCT_DEFINITION_CONTEXT ( 'detailed design', #12301, 'design' ) ;
#293 = AXIS2_PLACEMENT_3D ( 'NONE', #2741, #11961, #3821 ) ;
#294 = CIRCLE ( 'NONE', #504, 5.500000000000015099 ) ;
#295 = CIRCLE ( 'NONE', #1567, 239.8169934640465044 ) ;
#296 = CARTESIAN_POINT ( 'NONE',  ( 196.7513681799458709, 19.96883746115198122, -172.5787240287706936 ) ) ;
#297 = ADVANCED_FACE ( 'NONE', ( #1482 ), #8875, .F. ) ;
#298 = CARTESIAN_POINT ( 'NONE',  ( 227.3999999999999773, -0.1024105694488001289, -5.195143123655522110 ) ) ;
#299 =( REPRESENTATION_RELATIONSHIP ('NONE','NONE', #12019, #182 ) REPRESENTATION_RELATIONSHIP_WITH_TRANSFORMATION ( #9019 )SHAPE_REPRESENTATION_RELATIONSHIP( ) );
#300 = CARTESIAN_POINT ( 'NONE',  ( 0.000000000000000000, 0.000000000000000000, 0.000000000000000000 ) ) ;
#301 = DIRECTION ( 'NONE',  ( 0.000000000000000000, 1.000000000000000000, 0.000000000000000000 ) ) ;
#302 = CARTESIAN_POINT ( 'NONE',  ( -67.53249125288922983, 20.79694577634646890, 252.0229195836990925 ) ) ;
#303 = ORIENTED_EDGE ( 'NONE', *, *, #10671, .T. ) ;
#304 = CARTESIAN_POINT ( 'NONE',  ( 247.0684411393755795, 20.79694577634646535, 83.86521783953200782 ) ) ;
#305 = CIRCLE ( 'NONE', #7745, 5.099999999999993427 ) ;
#306 = EDGE_CURVE ( 'NONE', #11150, #4193, #9937, .T. ) ;
#307 = ORIENTED_EDGE ( 'NONE', *, *, #6492, .F. ) ;
#308 = CARTESIAN_POINT ( 'NONE',  ( 224.4939760857161843, 0.000000000000000000, 0.000000000000000000 ) ) ;
#309 = ORIENTED_EDGE ( 'NONE', *, *, #7048, .F. ) ;
#310 = ORIENTED_EDGE ( 'NONE', *, *, #416, .T. ) ;
#311 = AXIS2_PLACEMENT_3D ( 'NONE', #3386, #11606, #6408 ) ;
#312 = FACE_OUTER_BOUND ( 'NONE', #9369, .T. ) ;
#313 =( LENGTH_UNIT ( ) NAMED_UNIT ( * ) SI_UNIT ( .MILLI., .METRE. ) );
#314 = FACE_OUTER_BOUND ( 'NONE', #7559, .T. ) ;
#315 = CARTESIAN_POINT ( 'NONE',  ( 239.0883580245759390, 0.7438334345102074474, -3.420275401504354829 ) ) ;
#316 = CARTESIAN_POINT ( 'NONE',  ( -238.9443187634071535, 1.049086267421483143, -11.70307442294971345 ) ) ;
#317 = CARTESIAN_POINT ( 'NONE',  ( -243.1855895756006589, 7.483404894430283782, 9.380758043284854963 ) ) ;
#318 = DIRECTION ( 'NONE',  ( 0.6368676505102716101, 0.000000000000000000, 0.7709731485165527420 ) ) ;
#319 = ITEM_DEFINED_TRANSFORMATION ( 'NONE', 'NONE', #9331,  #805 ) ;
#320 = VERTEX_POINT ( 'NONE', #3539 ) ;
#321 = DIRECTION ( 'NONE',  ( 0.000000000000000000, 1.000000000000000000, 0.000000000000000000 ) ) ;
#322 = ORIENTED_EDGE ( 'NONE', *, *, #332, .F. ) ;
#323 = DIRECTION ( 'NONE',  ( 0.000000000000000000, 1.000000000000000000, 0.000000000000000000 ) ) ;
#324 = DIRECTION ( 'NONE',  ( 0.000000000000000000, 0.000000000000000000, -1.000000000000000000 ) ) ;
#325 = CIRCLE ( 'NONE', #4146, 5.500000000000005329 ) ;
#326 = CARTESIAN_POINT ( 'NONE',  ( 257.2112267038638151, 20.08915143297735995, 42.46883004693714980 ) ) ;
#327 = VERTEX_POINT ( 'NONE', #7610 ) ;
#328 = FACE_OUTER_BOUND ( 'NONE', #9057, .T. ) ;
#329 = CARTESIAN_POINT ( 'NONE',  ( -239.9450917581424960, 2.156506209390990136, -11.80463811257499884 ) ) ;
#330 = CARTESIAN_POINT ( 'NONE',  ( -239.9450917581424960, 2.156506209390990136, 11.80463811257499884 ) ) ;
#331 = FACE_OUTER_BOUND ( 'NONE', #10588, .T. ) ;
#332 = EDGE_CURVE ( 'NONE', #5214, #8298, #11654, .T. ) ;
#333 =( NAMED_UNIT ( * ) PLANE_ANGLE_UNIT ( ) SI_UNIT ( $, .RADIAN. ) );
#334 = PRODUCT ( 'Internal Mounting Flange Ring', 'Internal Mounting Flange Ring', '', ( #7461 ) ) ;
#335 = PRODUCT_CONTEXT ( 'NONE', #2943, 'mechanical' ) ;
#336 = CARTESIAN_POINT ( 'NONE',  ( 240.5727840947670870, 3.342302961292221486, -1.043131940273720026 ) ) ;
#337 = ITEM_DEFINED_TRANSFORMATION ( 'NONE', 'NONE', #10437,  #805 ) ;
#338 = CARTESIAN_POINT ( 'NONE',  ( -122.2593324768321992, 29.00000000000000000, 168.2755348299905052 ) ) ;
#339 = EDGE_LOOP ( 'NONE', ( #8886, #5505, #9, #5827 ) ) ;
#340 = CIRCLE ( 'NONE', #3522, 6.500000000000005329 ) ;
#341 = CARTESIAN_POINT ( 'NONE',  ( 226.6392846536925276, 19.96883745972948176, 130.8783844628973441 ) ) ;
#342 = CARTESIAN_POINT ( 'NONE',  ( -210.0000000000000000, 30.00000000000000000, -5.100000000000000533 ) ) ;
#343 = DIRECTION ( 'NONE',  ( 0.000000000000000000, 1.000000000000000000, 0.000000000000000000 ) ) ;
#344 = DIRECTION ( 'NONE',  ( 0.9135454576426033091, -0.4066576386751313277, 0.008016341293427268339 ) ) ;
#345 = DIRECTION ( 'NONE',  ( 0.000000000000000000, 0.000000000000000000, -1.000000000000000000 ) ) ;
#346 = ADVANCED_FACE ( 'NONE', ( #6298 ), #7414, .T. ) ;
#347 = LINE ( 'NONE', #4396, #11357 ) ;
#348 = CARTESIAN_POINT ( 'NONE',  ( -26.90145978217131884, -138.4705547276867321, 32.05991134143122423 ) ) ;
#349 = LINE ( 'NONE', #3328, #6709 ) ;
#350 = CONTEXT_DEPENDENT_SHAPE_REPRESENTATION ( #4909, #9223 ) ;
#351 = CARTESIAN_POINT ( 'NONE',  ( 240.5500529090736279, -3.279976618992322734, -1.225241158514834394 ) ) ;
#352 = CARTESIAN_POINT ( 'NONE',  ( -171.9542656377731475, -18.00000000000000000, -208.1627500994694344 ) ) ;
#353 = EDGE_LOOP ( 'NONE', ( #11784, #3307 ) ) ;
#354 = VERTEX_POINT ( 'NONE', #3337 ) ;
#355 = EDGE_CURVE ( 'NONE', #8227, #8752, #1859, .T. ) ;
#356 = FACE_OUTER_BOUND ( 'NONE', #2990, .T. ) ;
#357 = CARTESIAN_POINT ( 'NONE',  ( 235.1468102975488250, -18.00000000000000000, -194.2446334056325554 ) ) ;
#358 = CARTESIAN_POINT ( 'NONE',  ( -196.8887528216966132, 20.55460285140358678, -172.6991790949711287 ) ) ;
#359 = FACE_OUTER_BOUND ( 'NONE', #11465, .T. ) ;
#360 = PRODUCT_DEFINITION_SHAPE ( 'NONE', 'NONE',  #13163 ) ;
#361 = DIRECTION ( 'NONE',  ( -0.8660254037844364872, 0.000000000000000000, -0.5000000000000041078 ) ) ;
#362 = CARTESIAN_POINT ( 'NONE',  ( -240.4375400852135556, 3.701007121351563622, 11.16264886369179443 ) ) ;
#363 = DIRECTION ( 'NONE',  ( 0.5469441386039890496, 0.000000000000000000, -0.8371691043312220470 ) ) ;
#364 = EDGE_LOOP ( 'NONE', ( #8503, #2474 ) ) ;
#365 = CARTESIAN_POINT ( 'NONE',  ( 190.4297758776779688, 20.79694577634647246, -178.3611219674584163 ) ) ;
#366 = VERTEX_POINT ( 'NONE', #1547 ) ;
#367 = DIRECTION ( 'NONE',  ( -0.6368676505102707219, 0.000000000000000000, -0.7709731485165535192 ) ) ;
#368 = VERTEX_POINT ( 'NONE', #8676 ) ;
#369 = ORIENTED_EDGE ( 'NONE', *, *, #5052, .F. ) ;
#370 = EDGE_CURVE ( 'NONE', #690, #1431, #11004, .T. ) ;
#371 = EDGE_CURVE ( 'NONE', #12258, #9610, #11751, .T. ) ;
#372 = LINE ( 'NONE', #9371, #6679 ) ;
#373 = CARTESIAN_POINT ( 'NONE',  ( 221.6213872890270977, -19.00000000000000000, -190.2057062658400923 ) ) ;
#374 = CARTESIAN_POINT ( 'NONE',  ( 239.0381261355853724, 0.5585874493560030185, -3.455211367196914463 ) ) ;
#375 = EDGE_CURVE ( 'NONE', #2492, #808, #9229, .T. ) ;
#376 = CARTESIAN_POINT ( 'NONE',  ( -239.2060318623362321, 1.486384198450626526, -11.65560593358670260 ) ) ;
#377 = CYLINDRICAL_SURFACE ( 'NONE', #4954, 5.100000000000003197 ) ;
#378 = ITEM_DEFINED_TRANSFORMATION ( 'NONE', 'NONE', #9539,  #805 ) ;
#379 = VERTEX_POINT ( 'NONE', #7675 ) ;
#380 = DIRECTION ( 'NONE',  ( -0.000000000000000000, -1.000000000000000000, 0.000000000000000000 ) ) ;
#382 = ORIENTED_EDGE ( 'NONE', *, *, #554, .T. ) ;
#381 = AXIS2_PLACEMENT_3D ( 'NONE', #10792, #6742, #6676 ) ;
#383 = DIRECTION ( 'NONE',  ( 0.6368676505102707219, 0.000000000000000000, 0.7709731485165536302 ) ) ;
#384 = LINE ( 'NONE', #12452, #9582 ) ;
#385 = ADVANCED_FACE ( 'NONE', ( #12734 ), #10286, .F. ) ;
#386 = CARTESIAN_POINT ( 'NONE',  ( 178.2104428091929265, 20.08915143297737060, -190.2689011420770271 ) ) ;
#387 = DIRECTION ( 'NONE',  ( 0.000000000000000000, -1.000000000000000000, 0.000000000000000000 ) ) ;
#388 = CARTESIAN_POINT ( 'NONE',  ( -244.8267157023690004, 8.641841620762505727, -8.325778331754211337 ) ) ;
#389 = DIRECTION ( 'NONE',  ( 0.000000000000000000, 0.000000000000000000, 1.000000000000000000 ) ) ;
#390 = CARTESIAN_POINT ( 'NONE',  ( -240.6618454235819513, -4.173161342500063320, -10.98396364135015801 ) ) ;
#391 =( GEOMETRIC_REPRESENTATION_CONTEXT ( 3 ) GLOBAL_UNCERTAINTY_ASSIGNED_CONTEXT ( ( #7955 ) ) GLOBAL_UNIT_ASSIGNED_CONTEXT ( ( #11965, #7032, #5022 ) ) REPRESENTATION_CONTEXT ( 'NONE', 'WORKASPACE' ) );
#392 = CARTESIAN_POINT ( 'NONE',  ( -166.5596220099214690, -3.327561323230905366, -201.6321540179175713 ) ) ;
#393 = APPLICATION_PROTOCOL_DEFINITION ( 'draft international standard', 'automotive_design', 1998, #2333 ) ;
#394 = CARTESIAN_POINT ( 'NONE',  ( 227.3999999999999773, -0.1024105694488001289, -5.195143123655522110 ) ) ;
#395 = ITEM_DEFINED_TRANSFORMATION ( 'NONE', 'NONE', #12571,  #805 ) ;
#396 = B_SPLINE_CURVE_WITH_KNOTS ( 'NONE', 3,
 ( #120, #5441, #9444, #12376, #8383, #5564, #11439, #6316, #7439, #3497, #2434, #11511, #3229, #10634, #316, #12444, #9502, #1502, #2297, #10366, #3424, #12572, #7508, #376, #1376, #7310, #1308, #6515, #11576, #6574, #4424 ),
 .UNSPECIFIED., .F., .F.,
 ( 4, 2, 1, 1, 1, 2, 2, 2, 2, 1, 1, 2, 2, 2, 1, 1, 2, 2, 4 ),
 ( 0.5000762880526811172, 0.5039819420522705373, 0.5078875960518599575, 0.5156989040510386868, 0.5313215200493963675, 0.5625667520461116178, 0.6250572160395442278, 0.7500381440264094479, 0.7578494520255938394, 0.7656607600247783418, 0.7812833760231472358, 0.8125286080198849126, 0.8750190720133503852, 0.8789247260129398054, 0.8828303800125294476, 0.8906416880116931889, 0.9062643040100208935, 0.9375095360066760808, 1.000000000000000000 ),
 .UNSPECIFIED. ) ;
#397 = AXIS2_PLACEMENT_3D ( 'NONE', #3303, #10513, #5447 ) ;
#398 = AXIS2_PLACEMENT_3D ( 'NONE', #10071, #9274, #3936 ) ;
#399 = AXIS2_PLACEMENT_3D ( 'NONE', #6624, #2482, #10747 ) ;
#400 = DIRECTION ( 'NONE',  ( 0.000000000000000000, 1.000000000000000000, 0.000000000000000000 ) ) ;
#401 = ORIENTED_EDGE ( 'NONE', *, *, #140, .T. ) ;
#402 = CARTESIAN_POINT ( 'NONE',  ( -34.20858920445061102, 20.55460285115536934, 259.6535381498995321 ) ) ;
#403 = DIRECTION ( 'NONE',  ( 0.7709731485165535192, -0.000000000000000000, -0.6368676505102707219 ) ) ;
#404 = LINE ( 'NONE', #12663, #505 ) ;
#405 = CYLINDRICAL_SURFACE ( 'NONE', #4254, 11.75000000000000000 ) ;
#406 = CARTESIAN_POINT ( 'NONE',  ( -258.4638482596386098, 20.08915143297736705, 34.02434144668497851 ) ) ;
#407 = VECTOR ( 'NONE', #3982, 1000.000000000000114 ) ;
#408 = FACE_OUTER_BOUND ( 'NONE', #8960, .T. ) ;
#409 = DIRECTION ( 'NONE',  ( -0.8042250444015793809, 0.5538822189107471816, 0.2154914511802844823 ) ) ;
#410 = DIRECTION ( 'NONE',  ( 0.6368676505102707219, 0.000000000000000000, 0.7709731485165535192 ) ) ;
#411 = AXIS2_PLACEMENT_3D ( 'NONE', #8959, #7961, #12028 ) ;
#412 = CARTESIAN_POINT ( 'NONE',  ( 240.6009466513765176, -3.417710891889066627, 0.7616916526936037268 ) ) ;
#413 = AXIS2_PLACEMENT_3D ( 'NONE', #9466, #8658, #6404 ) ;
#414 = CARTESIAN_POINT ( 'NONE',  ( 0.000000000000000000, -13.19999999999999929, 0.000000000000000000 ) ) ;
#415 = EDGE_LOOP ( 'NONE', ( #4979, #4482 ) ) ;
#416 = EDGE_CURVE ( 'NONE', #3329, #13033, #7804, .T. ) ;
#417 = ORIENTED_EDGE ( 'NONE', *, *, #10700, .F. ) ;
#418 = ADVANCED_FACE ( 'NONE', ( #10744, #4871, #681, #11821, #9730, #1615, #2543, #12876, #6620, #1747, #10675, #555, #13009 ), #3605, .F. ) ;
#419 = VECTOR ( 'NONE', #10160, 1000.000000000000000 ) ;
#420 = CARTESIAN_POINT ( 'NONE',  ( 0.000000000000000000, -20.69999999999999929, 0.000000000000000000 ) ) ;
#421 = DIRECTION ( 'NONE',  ( 0.000000000000000000, -1.000000000000000000, 0.000000000000000000 ) ) ;
#422 = B_SPLINE_CURVE_WITH_KNOTS ( 'NONE', 3,
 ( #8574, #10632, #5371, #1500, #4556, #3352, #6315, #2239, #11641, #2496, #2295, #7568, #6573, #3423, #441, #6379, #10365, #12442, #4490, #4368, #9501, #315, #7375, #5563, #10436, #374, #8447, #12501, #7437 ),
 .UNSPECIFIED., .F., .F.,
 ( 4, 2, 2, 1, 1, 2, 2, 2, 1, 1, 2, 2, 2, 1, 2, 2, 4 ),
 ( 0.000000000000000000, 0.06264877319316634885, 0.09397315978975546991, 0.1096353530880500721, 0.1174664497371907118, 0.1213819980617677902, 0.1252975463863448546, 0.1879463195796756692, 0.2192707061763410903, 0.2349328994746693877, 0.2427639961238378385, 0.2505950927730062894, 0.3132438659663454028, 0.3445682525630119897, 0.3602304458613453941, 0.3758926391596786876, 0.5011901855463575250 ),
 .UNSPECIFIED. ) ;
#423 = CARTESIAN_POINT ( 'NONE',  ( 130.8783844624215931, 19.96883746229290679, 226.6392846534563716 ) ) ;
#424 = FACE_OUTER_BOUND ( 'NONE', #2937, .T. ) ;
#425 = CARTESIAN_POINT ( 'NONE',  ( 0.000000000000000000, 0.000000000000000000, 0.000000000000000000 ) ) ;
#426 =( REPRESENTATION_RELATIONSHIP ('NONE','NONE', #12019, #5191 ) REPRESENTATION_RELATIONSHIP_WITH_TRANSFORMATION ( #2987 )SHAPE_REPRESENTATION_RELATIONSHIP( ) );
#427 = CARTESIAN_POINT ( 'NONE',  ( -286.5445428119863323, -30.00000000000000000, -22.67813138875635204 ) ) ;
#428 = EDGE_CURVE ( 'NONE', #612, #7121, #6260, .T. ) ;
#429 = DIRECTION ( 'NONE',  ( 1.000000000000000000, 0.000000000000000000, 0.000000000000000000 ) ) ;
#430 = AXIS2_PLACEMENT_3D ( 'NONE', #11339, #3065, #7146 ) ;
#431 = VERTEX_POINT ( 'NONE', #8744 ) ;
#432 = CARTESIAN_POINT ( 'NONE',  ( 91.90986972409962164, 20.79694577634646535, -244.1900186690935470 ) ) ;
#433 = AXIS2_PLACEMENT_3D ( 'NONE', #11650, #1512, #3568 ) ;
#434 = ORIENTED_EDGE ( 'NONE', *, *, #4249, .F. ) ;
#435 = DIRECTION ( 'NONE',  ( -0.000000000000000000, -1.000000000000000000, 0.000000000000000000 ) ) ;
#436 = EDGE_LOOP ( 'NONE', ( #2663, #922, #6967, #12561 ) ) ;
#437 = EDGE_LOOP ( 'NONE', ( #12968, #8052, #6929, #11620 ) ) ;
#438 = CARTESIAN_POINT ( 'NONE',  ( 171.9542656377731191, 19.00000000000000000, 208.1627500994694628 ) ) ;
#439 = PRODUCT ( 'Slewing Ring High Pressure Lip Seals Top', 'Slewing Ring High Pressure Lip Seals Top', '', ( #335 ) ) ;
#440 = DIRECTION ( 'NONE',  ( 0.000000000000000000, 0.9998057603070480415, -0.01970892327970899874 ) ) ;
#441 = CARTESIAN_POINT ( 'NONE',  ( 239.2626306339685982, 1.161280184642565771, -3.302084438317430148 ) ) ;
#442 = AXIS2_PLACEMENT_3D ( 'NONE', #1341, #5410, #6482 ) ;
#443 = DIRECTION ( 'NONE',  ( 0.000000000000000000, 0.000000000000000000, 1.000000000000000000 ) ) ;
#444 = SURFACE_STYLE_USAGE ( .BOTH. , #9562 ) ;
#445 = ADVANCED_FACE ( 'NONE', ( #12807 ), #6891, .F. ) ;
#446 = EDGE_CURVE ( 'NONE', #12435, #9116, #11362, .T. ) ;
#447 = ITEM_DEFINED_TRANSFORMATION ( 'NONE', 'NONE', #1032,  #805 ) ;
#448 = CIRCLE ( 'NONE', #4682, 5.499999999999998224 ) ;
#449 = ORIENTED_EDGE ( 'NONE', *, *, #355, .T. ) ;
#450 = DIRECTION ( 'NONE',  ( 0.000000000000000000, 1.000000000000000000, 0.000000000000000000 ) ) ;
#451 = ORIENTED_EDGE ( 'NONE', *, *, #6978, .F. ) ;
#452 = CARTESIAN_POINT ( 'NONE',  ( -31.19222893191933821, -29.00000000000000000, 286.4438302234618163 ) ) ;
#453 = AXIS2_PLACEMENT_3D ( 'NONE', #11170, #7172, #2039 ) ;
#454 = CARTESIAN_POINT ( 'NONE',  ( 182.4625818711949137, -29.00000000000000000, 220.8838070499906507 ) ) ;
#455 = PLANE ( 'NONE',  #2846 ) ;
#456 = CARTESIAN_POINT ( 'NONE',  ( 0.000000000000000000, 25.50000000000000000, 0.000000000000000000 ) ) ;
#457 = CARTESIAN_POINT ( 'NONE',  ( -229.8300945347042159, 7.760684502249874051, 8.855560954721353184 ) ) ;
#458 = AXIS2_PLACEMENT_3D ( 'NONE', #522, #1584, #5646 ) ;
#459 = CARTESIAN_POINT ( 'NONE',  ( -247.5810890924702790, -9.727605306517407513, -7.026623146109774787 ) ) ;
#460 = ADVANCED_FACE ( 'NONE', ( #6754 ), #4532, .F. ) ;
#461 = DIRECTION ( 'NONE',  ( 0.4503334343941581830, -0.7071067811865450192, 0.5451603414288000993 ) ) ;
#462 = APPLICATION_PROTOCOL_DEFINITION ( 'draft international standard', 'automotive_design', 1998, #914 ) ;
#463 = CARTESIAN_POINT ( 'NONE',  ( 71.82423009839129691, 30.00000000000000000, -197.3354503650404865 ) ) ;
#464 = EDGE_CURVE ( 'NONE', #12890, #3753, #4734, .T. ) ;
#465 = CIRCLE ( 'NONE', #8338, 6.500000000000005329 ) ;
#466 = DIRECTION ( 'NONE',  ( 0.000000000000000000, 0.000000000000000000, 1.000000000000000000 ) ) ;
#467 = ORIENTED_EDGE ( 'NONE', *, *, #10070, .F. ) ;
#468 = VERTEX_POINT ( 'NONE', #9561 ) ;
#469 = CARTESIAN_POINT ( 'NONE',  ( -130.8783844626380812, 19.96883746054828279, -226.6392846538615231 ) ) ;
#470 = DIRECTION ( 'NONE',  ( 0.000000000000000000, 0.000000000000000000, 1.000000000000000000 ) ) ;
#471 = FACE_OUTER_BOUND ( 'NONE', #1035, .T. ) ;
#472 = APPLICATION_CONTEXT ( 'automotive_design' ) ;
#473 = CIRCLE ( 'NONE', #10902, 5.500000000000005329 ) ;
#474 = DIRECTION ( 'NONE',  ( 0.000000000000000000, 0.9998057603070481525, -0.01970892327970900221 ) ) ;
#475 = CARTESIAN_POINT ( 'NONE',  ( -17.05322212017849282, 20.08915143297736705, 260.1353576186480154 ) ) ;
#476 = CARTESIAN_POINT ( 'NONE',  ( -240.1208361041844910, 2.772967769358964940, -11.41810622433052025 ) ) ;
#477 = DIRECTION ( 'NONE',  ( -0.4226182617407033271, 0.000000000000000000, 0.9063077870366481603 ) ) ;
#478 = CARTESIAN_POINT ( 'NONE',  ( 229.9948475045917462, 3.144455231364676084, -1.553991905490903713 ) ) ;
#479 = CIRCLE ( 'NONE', #696, 5.500000000000005329 ) ;
#480 = ITEM_DEFINED_TRANSFORMATION ( 'NONE', 'NONE', #5978,  #805 ) ;
#481 = AXIS2_PLACEMENT_3D ( 'NONE', #1897, #9541, #12361 ) ;
#482 = FACE_OUTER_BOUND ( 'NONE', #9432, .T. ) ;
#483 = DIRECTION ( 'NONE',  ( 8.659560562354939021E-17, 0.7071067811865470176, -0.7071067811865480168 ) ) ;
#484 = AXIS2_PLACEMENT_3D ( 'NONE', #2681, #9957, #3755 ) ;
#485 = ORIENTED_EDGE ( 'NONE', *, *, #1724, .F. ) ;
#486 = ORIENTED_EDGE ( 'NONE', *, *, #7148, .F. ) ;
#487 =( REPRESENTATION_RELATIONSHIP ('NONE','NONE', #12019, #182 ) REPRESENTATION_RELATIONSHIP_WITH_TRANSFORMATION ( #8354 )SHAPE_REPRESENTATION_RELATIONSHIP( ) );
#488 = CARTESIAN_POINT ( 'NONE',  ( -239.9450917581424960, 2.156506209390990136, 11.80463811257499884 ) ) ;
#489 = CARTESIAN_POINT ( 'NONE',  ( 235.0999999999999943, -1.949621232598743648, 0.03843240039543278225 ) ) ;
#490 = AXIS2_PLACEMENT_3D ( 'NONE', #7345, #7278, #6481 ) ;
#491 = CARTESIAN_POINT ( 'NONE',  ( 252.9796497720284094, 20.55460285130353881, -67.76049180262273808 ) ) ;
#492 = DIRECTION ( 'NONE',  ( 0.000000000000000000, 0.000000000000000000, 1.000000000000000000 ) ) ;
#493 = DIRECTION ( 'NONE',  ( -0.5735764363510499342, 0.000000000000000000, 0.8191520442889893561 ) ) ;
#494 = DIRECTION ( 'NONE',  ( 0.5469441386039890496, 0.000000000000000000, -0.8371691043312220470 ) ) ;
#495 = CARTESIAN_POINT ( 'NONE',  ( -225.9597979674043415, 20.79694577634646535, -130.4544329367272724 ) ) ;
#496 = ADVANCED_FACE ( 'NONE', ( #4803 ), #9936, .T. ) ;
#497 = VERTEX_POINT ( 'NONE', #8948 ) ;
#498 = CARTESIAN_POINT ( 'NONE',  ( 260.3553053170167004, 20.79694577634646535, -17.06764083276446087 ) ) ;
#499 = ORIENTED_EDGE ( 'NONE', *, *, #7130, .T. ) ;
#500 = DIRECTION ( 'NONE',  ( -0.6368676505102737195, 0.000000000000000000, -0.7709731485165509657 ) ) ;
#501 = ORIENTED_EDGE ( 'NONE', *, *, #11632, .T. ) ;
#502 = ORIENTED_EDGE ( 'NONE', *, *, #3627, .F. ) ;
#503 = AXIS2_PLACEMENT_3D ( 'NONE', #10733, #3595, #9864 ) ;
#504 = AXIS2_PLACEMENT_3D ( 'NONE', #4431, #380, #12767 ) ;
#505 = VECTOR ( 'NONE', #4454, 1000.000000000000000 ) ;
#506 = DIRECTION ( 'NONE',  ( 0.000000000000000000, 0.000000000000000000, -1.000000000000000000 ) ) ;
#507 = DIRECTION ( 'NONE',  ( -0.000000000000000000, -1.000000000000000000, 0.000000000000000000 ) ) ;
#508 = AXIS2_PLACEMENT_3D ( 'NONE', #7743, #6880, #10941 ) ;
#509 = CARTESIAN_POINT ( 'NONE',  ( 185.9653539490014111, -30.00000000000000000, 225.1241593668316625 ) ) ;
#510 = DIRECTION ( 'NONE',  ( 0.000000000000000000, -1.000000000000000000, 0.000000000000000000 ) ) ;
#511 = FACE_OUTER_BOUND ( 'NONE', #4843, .T. ) ;
#512 = EDGE_CURVE ( 'NONE', #4498, #11239, #1570, .T. ) ;
#513 = AXIS2_PLACEMENT_3D ( 'NONE', #12749, #7424, #11499 ) ;
#514 = ORIENTED_EDGE ( 'NONE', *, *, #864, .T. ) ;
#515 = DIRECTION ( 'NONE',  ( -1.000000000000000000, 0.000000000000000000, 0.000000000000000000 ) ) ;
#516 = ORIENTED_EDGE ( 'NONE', *, *, #3019, .F. ) ;
#517 = CARTESIAN_POINT ( 'NONE',  ( -243.5599937619014952, 7.782121691016424592, -8.802892736592429657 ) ) ;
#518 = CARTESIAN_POINT ( 'NONE',  ( 159.3442861576696998, -25.50000000000000000, 192.8974817588417352 ) ) ;
#519 = EDGE_CURVE ( 'NONE', #3488, #167, #5232, .T. ) ;
#520 = DIRECTION ( 'NONE',  ( 0.000000000000000000, -1.000000000000000000, 0.000000000000000000 ) ) ;
#521 = EDGE_CURVE ( 'NONE', #5366, #4133, #12274, .T. ) ;
#522 = CARTESIAN_POINT ( 'NONE',  ( 0.000000000000000000, 19.00000000000000000, 250.7029414592220178 ) ) ;
#523 = CARTESIAN_POINT ( 'NONE',  ( -239.4244912090118191, 1.754035804298239798, 11.87111434752389272 ) ) ;
#524 = DIRECTION ( 'NONE',  ( 0.000000000000000000, 0.000000000000000000, -1.000000000000000000 ) ) ;
#525 = CARTESIAN_POINT ( 'NONE',  ( -247.9423986614758348, -9.805815554863000827, 6.917079555584196626 ) ) ;
#526 = DIRECTION ( 'NONE',  ( -0.6368676505102698338, 0.000000000000000000, -0.7709731485165541853 ) ) ;
#527 = CARTESIAN_POINT ( 'NONE',  ( -229.9856741818797445, 11.72241588658361167, -2.593326906271713916 ) ) ;
#528 = AXIS2_PLACEMENT_3D ( 'NONE', #5634, #4617, #3756 ) ;
#529 = ITEM_DEFINED_TRANSFORMATION ( 'NONE', 'NONE', #8955,  #805 ) ;
#530 = VECTOR ( 'NONE', #9464, 1000.000000000000227 ) ;
#531 = ORIENTED_EDGE ( 'NONE', *, *, #1101, .F. ) ;
#532 = ORIENTED_EDGE ( 'NONE', *, *, #8990, .T. ) ;
#533 = CARTESIAN_POINT ( 'NONE',  ( -122.2593324768359935, 29.00000000000000000, -162.7755348299880040 ) ) ;
#534 = VERTEX_POINT ( 'NONE', #9137 ) ;
#535 = EDGE_CURVE ( 'NONE', #8515, #6953, #11631, .T. ) ;
#536 = CARTESIAN_POINT ( 'NONE',  ( -226.6392846536229229, 19.96883746130017911, -130.8783844628770794 ) ) ;
#537 = ADVANCED_FACE ( 'NONE', ( #2993 ), #3527, .T. ) ;
#538 = CARTESIAN_POINT ( 'NONE',  ( -290.6841825403030839, -19.00000000000000000, -27.68945685411394919 ) ) ;
#539 = CARTESIAN_POINT ( 'NONE',  ( 27.68945685411497593, -19.00000000000000000, -290.6841825403026291 ) ) ;
#540 = DIRECTION ( 'NONE',  ( 1.000000000000000000, 0.000000000000000000, 0.000000000000000000 ) ) ;
#541 = CIRCLE ( 'NONE', #9685, 0.7999999999999999334 ) ;
#542 = CARTESIAN_POINT ( 'NONE',  ( -241.2764277293246664, 5.294572826602574445, 10.76882343127053865 ) ) ;
#543 = EDGE_CURVE ( 'NONE', #8768, #1281, #5197, .T. ) ;
#544 = DIRECTION ( 'NONE',  ( 0.000000000000000000, 0.7071067811865280328, 0.7071067811865670016 ) ) ;
#545 = DIRECTION ( 'NONE',  ( 0.2588190451025179639, 0.000000000000000000, 0.9659258262890690894 ) ) ;
#546 = CARTESIAN_POINT ( 'NONE',  ( 229.9884017560907807, 2.634578860511305631, -2.315394940318573624 ) ) ;
#547 = CARTESIAN_POINT ( 'NONE',  ( -241.1581829739467366, -5.108108803544517684, -10.85886904366963712 ) ) ;
#548 = AXIS2_PLACEMENT_3D ( 'NONE', #622, #3812, #2548 ) ;
#549 = AXIS2_PLACEMENT_3D ( 'NONE', #4500, #3705, #6585 ) ;
#550 = DIRECTION ( 'NONE',  ( 8.659560562354926695E-17, 0.7071067811865480168, -0.7071067811865470176 ) ) ;
#551 = EDGE_LOOP ( 'NONE', ( #10115, #7698 ) ) ;
#552 = VERTEX_POINT ( 'NONE', #6014 ) ;
#553 = CARTESIAN_POINT ( 'NONE',  ( 7.347880794884118750E-16, 29.00000000000000000, 202.4999999999999716 ) ) ;
#554 = EDGE_CURVE ( 'NONE', #12610, #6169, #9285, .T. ) ;
#555 = FACE_BOUND ( 'NONE', #1673, .T. ) ;
#556 = CARTESIAN_POINT ( 'NONE',  ( 226.7975291061089820, 20.55460285063310621, -130.9697226050975019 ) ) ;
#557 = CIRCLE ( 'NONE', #5230, 250.7000000000000171 ) ;
#558 = DIRECTION ( 'NONE',  ( 0.6368676505102737195, 0.000000000000000000, 0.7709731485165509657 ) ) ;
#559 = DIRECTION ( 'NONE',  ( -0.6427876096865430267, 0.000000000000000000, 0.7660444431189749048 ) ) ;
#560 = FACE_OUTER_BOUND ( 'NONE', #6115, .T. ) ;
#561 = CARTESIAN_POINT ( 'NONE',  ( 182.4625818711949137, -19.00000000000000000, 220.8838070499906223 ) ) ;
#562 = ORIENTED_EDGE ( 'NONE', *, *, #6556, .F. ) ;
#563 = FACE_OUTER_BOUND ( 'NONE', #5860, .T. ) ;
#564 = VERTEX_POINT ( 'NONE', #6140 ) ;
#565 = CYLINDRICAL_SURFACE ( 'NONE', #12328, 254.1999999999999886 ) ;
#566 = ORIENTED_EDGE ( 'NONE', *, *, #6725, .F. ) ;
#567 = ORIENTED_EDGE ( 'NONE', *, *, #4107, .F. ) ;
#568 = ORIENTED_EDGE ( 'NONE', *, *, #1085, .T. ) ;
#569 = DIRECTION ( 'NONE',  ( 0.000000000000000000, 0.000000000000000000, 1.000000000000000000 ) ) ;
#570 = FACE_OUTER_BOUND ( 'NONE', #8193, .T. ) ;
#571 = DIRECTION ( 'NONE',  ( -0.000000000000000000, -1.000000000000000000, 0.000000000000000000 ) ) ;
#572 = ORIENTED_EDGE ( 'NONE', *, *, #10231, .F. ) ;
#573 = DIRECTION ( 'NONE',  ( 0.000000000000000000, 0.000000000000000000, 1.000000000000000000 ) ) ;
#574 = EDGE_LOOP ( 'NONE', ( #7370, #1369 ) ) ;
#575 = PRODUCT_DEFINITION_SHAPE ( 'NONE', 'NONE',  #13180 ) ;
#576 = CARTESIAN_POINT ( 'NONE',  ( -244.2253259530033063, 8.263305842943061919, -8.353459642338018298 ) ) ;
#577 = ORIENTED_EDGE ( 'NONE', *, *, #3546, .T. ) ;
#578 = ADVANCED_FACE ( 'NONE', ( #10195 ), #8912, .T. ) ;
#579 = EDGE_CURVE ( 'NONE', #3020, #10014, #12322, .T. ) ;
#580 = CARTESIAN_POINT ( 'NONE',  ( 240.3599429726558299, -2.697249171038460069, -2.233886006210043629 ) ) ;
#581 = DIRECTION ( 'NONE',  ( -0.000000000000000000, -1.000000000000000000, 0.000000000000000000 ) ) ;
#582 = CARTESIAN_POINT ( 'NONE',  ( 227.3999999999999773, -4.550331206106116078, -2.508881407069070590 ) ) ;
#583 = DIRECTION ( 'NONE',  ( 0.000000000000000000, 1.000000000000000000, 0.000000000000000000 ) ) ;
#584 = PRODUCT_DEFINITION_SHAPE ( 'NONE', 'NONE',  #13121 ) ;
#585 = AXIS2_PLACEMENT_3D ( 'NONE', #11911, #2760, #6847 ) ;
#586 = DIRECTION ( 'NONE',  ( 1.000000000000000000, 0.000000000000000000, 0.000000000000000000 ) ) ;
#587 = PRODUCT_RELATED_PRODUCT_CATEGORY ( 'part', '', ( #1393 ) ) ;
#588 = DIRECTION ( 'NONE',  ( 0.000000000000000000, 1.000000000000000000, 0.000000000000000000 ) ) ;
#589 = ORIENTED_EDGE ( 'NONE', *, *, #10916, .T. ) ;
#590 = ORIENTED_EDGE ( 'NONE', *, *, #10836, .F. ) ;
#591 = CARTESIAN_POINT ( 'NONE',  ( -0.000000000000000000, -3.165711975795909891E-14, 0.000000000000000000 ) ) ;
#592 = ORIENTED_EDGE ( 'NONE', *, *, #10942, .T. ) ;
#593 = AXIS2_PLACEMENT_3D ( 'NONE', #7570, #8695, #1632 ) ;
#594 = CARTESIAN_POINT ( 'NONE',  ( 115.7315435902013263, 19.96883745981483926, -234.7354397754176318 ) ) ;
#595 = CARTESIAN_POINT ( 'NONE',  ( 0.000000000000000000, 24.75600756274008063, -251.5674242726970817 ) ) ;
#596 = CARTESIAN_POINT ( 'NONE',  ( 0.000000000000000000, 9.830508068699479907, 0.000000000000000000 ) ) ;
#597 =( REPRESENTATION_RELATIONSHIP ('NONE','NONE', #12019, #5191 ) REPRESENTATION_RELATIONSHIP_WITH_TRANSFORMATION ( #337 )SHAPE_REPRESENTATION_RELATIONSHIP( ) );
#598 = DIRECTION ( 'NONE',  ( -0.000000000000000000, -1.000000000000000000, 0.000000000000000000 ) ) ;
#599 = CARTESIAN_POINT ( 'NONE',  ( -0.000000000000000000, -11.79660968244695951, 0.000000000000000000 ) ) ;
#600 = DIRECTION ( 'NONE',  ( -0.000000000000000000, -1.000000000000000000, 0.000000000000000000 ) ) ;
#601 = CARTESIAN_POINT ( 'NONE',  ( -24.00488622054064081, -138.4705547276867321, -34.28253040793676831 ) ) ;
#602 = ADVANCED_FACE ( 'NONE', ( #12211 ), #1031, .T. ) ;
#603 = DIRECTION ( 'NONE',  ( -0.000000000000000000, -1.000000000000000000, 0.000000000000000000 ) ) ;
#604 = AXIS2_PLACEMENT_3D ( 'NONE', #8620, #4664, #3604 ) ;
#605 = CONTEXT_DEPENDENT_SHAPE_REPRESENTATION ( #6535, #11980 ) ;
#606 = AXIS2_PLACEMENT_3D ( 'NONE', #8974, #3743, #1946 ) ;
#607 = EDGE_CURVE ( 'NONE', #4062, #10624, #1004, .T. ) ;
#608 = CARTESIAN_POINT ( 'NONE',  ( -248.8555022324198092, 10.14371006999433789, -5.930260235961137383 ) ) ;
#609 = CARTESIAN_POINT ( 'NONE',  ( -241.2764277293045438, -5.294572826571302571, -10.76882343128240471 ) ) ;
#610 = CARTESIAN_POINT ( 'NONE',  ( 197.8197553893920144, 18.00000000000000000, 64.27553482998850143 ) ) ;
#611 = EDGE_LOOP ( 'NONE', ( #7240, #5539, #12625, #572 ) ) ;
#612 = VERTEX_POINT ( 'NONE', #7075 ) ;
#613 = DIRECTION ( 'NONE',  ( -0.7709731485165535192, 0.000000000000000000, 0.6368676505102708330 ) ) ;
#614 = AXIS2_PLACEMENT_3D ( 'NONE', #8258, #6261, #383 ) ;
#615 = CIRCLE ( 'NONE', #3368, 3.000000000000000000 ) ;
#616 = VECTOR ( 'NONE', #8753, 1000.000000000000000 ) ;
#617 = CARTESIAN_POINT ( 'NONE',  ( -1.009183486025028462E-12, 20.55460285106647689, 261.3381329044966606 ) ) ;
#618 = AXIS2_PLACEMENT_3D ( 'NONE', #4311, #11452, #1830 ) ;
#619 = DIRECTION ( 'NONE',  ( -0.6368676505102706109, 0.000000000000000000, -0.7709731485165535192 ) ) ;
#620 = DIRECTION ( 'NONE',  ( -0.3420201433256631063, 0.000000000000000000, -0.9396926207859106484 ) ) ;
#621 = DIRECTION ( 'NONE',  ( 0.000000000000000000, 1.000000000000000000, 0.000000000000000000 ) ) ;
#622 = CARTESIAN_POINT ( 'NONE',  ( 0.000000000000000000, -2.957522019940860139E-14, 0.000000000000000000 ) ) ;
#623 = AXIS2_PLACEMENT_3D ( 'NONE', #5398, #3520, #1527 ) ;
#624 = EDGE_CURVE ( 'NONE', #1954, #9495, #12952, .T. ) ;
#625 = ORIENTED_EDGE ( 'NONE', *, *, #1514, .F. ) ;
#626 = AXIS2_PLACEMENT_3D ( 'NONE', #7112, #7979, #4970 ) ;
#627 = DIRECTION ( 'NONE',  ( 0.000000000000000000, 1.000000000000000000, 0.000000000000000000 ) ) ;
#628 = ORIENTED_EDGE ( 'NONE', *, *, #6008, .T. ) ;
#629 = ORIENTED_EDGE ( 'NONE', *, *, #6249, .T. ) ;
#630 = CARTESIAN_POINT ( 'NONE',  ( 137.6665579279354006, 20.08915143297736350, 221.3800702329288299 ) ) ;
#631 = ORIENTED_EDGE ( 'NONE', *, *, #8325, .T. ) ;
#632 = AXIS2_PLACEMENT_3D ( 'NONE', #23, #5012, #3948 ) ;
#633 = CARTESIAN_POINT ( 'NONE',  ( 140.0242476638101152, -30.00000000000000000, -251.1826895432237166 ) ) ;
#634 = DIRECTION ( 'NONE',  ( 0.000000000000000000, 0.000000000000000000, 1.000000000000000000 ) ) ;
#635 = FACE_OUTER_BOUND ( 'NONE', #6751, .T. ) ;
#636 = CIRCLE ( 'NONE', #9776, 6.500000000000005329 ) ;
#637 = CARTESIAN_POINT ( 'NONE',  ( -27.68945685411286561, -30.00000000000000000, 290.6841825403027997 ) ) ;
#638 = CARTESIAN_POINT ( 'NONE',  ( -247.4721532356705040, 9.698102444925263299, 6.633777139661048317 ) ) ;
#639 = CIRCLE ( 'NONE', #9812, 5.100000000000003197 ) ;
#640 = EDGE_LOOP ( 'NONE', ( #3400, #6010, #3951, #10562, #8054 ) ) ;
#641 = DIRECTION ( 'NONE',  ( 0.000000000000000000, -1.000000000000000000, 0.000000000000000000 ) ) ;
#642 = ORIENTED_EDGE ( 'NONE', *, *, #9370, .T. ) ;
#643 = CARTESIAN_POINT ( 'NONE',  ( -242.9854649084194023, 7.295305385232032869, -9.211094753746992936 ) ) ;
#644 = VERTEX_POINT ( 'NONE', #944 ) ;
#645 = CIRCLE ( 'NONE', #5753, 1.750000000000000000 ) ;
#646 = CARTESIAN_POINT ( 'NONE',  ( 122.2593324768346008, 18.00000000000000000, 168.2755348299889988 ) ) ;
#647 = AXIS2_PLACEMENT_3D ( 'NONE', #5936, #7930, #1737 ) ;
#648 = DIRECTION ( 'NONE',  ( 0.6368676505102716101, 0.000000000000000000, 0.7709731485165527420 ) ) ;
#649 = CARTESIAN_POINT ( 'NONE',  ( 0.000000000000000000, -2.957522019940860139E-14, -241.5000000000000000 ) ) ;
#650 = CARTESIAN_POINT ( 'NONE',  ( -230.0000324180956568, 11.75063456719393606, -0.7654011193310154004 ) ) ;
#651 = CONICAL_SURFACE ( 'NONE', #1504, 5.099999999999993427, 0.7853981633974461696 ) ;
#652 = CARTESIAN_POINT ( 'NONE',  ( -240.6982673023520647, -4.277714796963365984, 11.21297710688243399 ) ) ;
#653 = DIRECTION ( 'NONE',  ( 1.000000000000000000, 0.000000000000000000, 0.000000000000000000 ) ) ;
#654 = ORIENTED_EDGE ( 'NONE', *, *, #2803, .T. ) ;
#655 = EDGE_CURVE ( 'NONE', #11681, #11485, #6209, .T. ) ;
#656 = DIRECTION ( 'NONE',  ( -0.4503334343941582940, -0.7071067811865450192, -0.5451603414288000993 ) ) ;
#657 = EDGE_CURVE ( 'NONE', #926, #2842, #5947, .T. ) ;
#658 = CONTEXT_DEPENDENT_SHAPE_REPRESENTATION ( #1958, #1316 ) ;
#659 = TOROIDAL_SURFACE ( 'NONE', #5728, 241.5000000000000000, 2.500000000000000000 ) ;
#660 = ORIENTED_EDGE ( 'NONE', *, *, #9431, .T. ) ;
#661 = ORIENTED_EDGE ( 'NONE', *, *, #5302, .F. ) ;
#662 = DIRECTION ( 'NONE',  ( 0.000000000000000000, -1.000000000000000000, 0.000000000000000000 ) ) ;
#663 = EDGE_LOOP ( 'NONE', ( #7219, #7167, #8642, #12298 ) ) ;
#664 = CARTESIAN_POINT ( 'NONE',  ( -261.3381329044966606, 20.55460285116648933, 17.10461161605900671 ) ) ;
#665 = FACE_BOUND ( 'NONE', #7591, .T. ) ;
#666 = DIRECTION ( 'NONE',  ( -0.4503334343941627904, -0.7071067811865381358, -0.5451603414288054283 ) ) ;
#667 = CARTESIAN_POINT ( 'NONE',  ( -287.1814104624966149, -19.00000000000000000, -23.44910453727290189 ) ) ;
#668 = CARTESIAN_POINT ( 'NONE',  ( 0.000000000000000000, 0.000000000000000000, 0.000000000000000000 ) ) ;
#669 = CARTESIAN_POINT ( 'NONE',  ( -240.7195678459729038, 4.326096554678287021, 11.19626641897951913 ) ) ;
#670 = CARTESIAN_POINT ( 'NONE',  ( -229.2637990951503753, -18.00000000000000000, 180.9540284836414514 ) ) ;
#671 = CARTESIAN_POINT ( 'NONE',  ( 2.922456606246464600E-13, -138.4705547276867321, -41.85124196045095601 ) ) ;
#672 = CARTESIAN_POINT ( 'NONE',  ( -229.9566917300585942, -10.87227007594808192, -4.504975736512506046 ) ) ;
#673 = VECTOR ( 'NONE', #3157, 1000.000000000000000 ) ;
#674 = CARTESIAN_POINT ( 'NONE',  ( -249.7825649081718780, 11.59499477621177910, 1.902498382194837578 ) ) ;
#675 = CARTESIAN_POINT ( 'NONE',  ( 0.000000000000000000, 2.772967769359004908, -240.3921568627450256 ) ) ;
#676 = ORIENTED_EDGE ( 'NONE', *, *, #6226, .T. ) ;
#677 = DIRECTION ( 'NONE',  ( 0.000000000000000000, 0.000000000000000000, -1.000000000000000000 ) ) ;
#678 = VERTEX_POINT ( 'NONE', #11072 ) ;
#679 = ORIENTED_EDGE ( 'NONE', *, *, #4416, .T. ) ;
#680 = DIRECTION ( 'NONE',  ( 0.000000000000000000, 0.9998057603070481525, -0.01970892327970899874 ) ) ;
#681 = FACE_BOUND ( 'NONE', #2232, .T. ) ;
#682 = ADVANCED_FACE ( 'NONE', ( #146 ), #11138, .F. ) ;
#683 = EDGE_CURVE ( 'NONE', #1246, #5570, #3794, .T. ) ;
#684 = CARTESIAN_POINT ( 'NONE',  ( -84.02568524195829980, 20.79694577620390916, -247.4557548102065141 ) ) ;
#685 = DIRECTION ( 'NONE',  ( 0.000000000000000000, 1.000000000000000000, 0.000000000000000000 ) ) ;
#686 = CARTESIAN_POINT ( 'NONE',  ( 0.000000000000000000, 0.000000000000000000, 0.000000000000000000 ) ) ;
#687 = CARTESIAN_POINT ( 'NONE',  ( 240.3826708216974737, -2.772967769359219847, 2.135567781667135012 ) ) ;
#688 = AXIS2_PLACEMENT_3D ( 'NONE', #9443, #1239, #11509 ) ;
#689 = CARTESIAN_POINT ( 'NONE',  ( -290.6841825403030839, -30.00000000000000000, -27.68945685411394919 ) ) ;
#690 = VERTEX_POINT ( 'NONE', #81 ) ;
#691 = VECTOR ( 'NONE', #2042, 1000.000000000000000 ) ;
#692 = LINE ( 'NONE', #9946, #1305 ) ;
#693 = B_SPLINE_CURVE_WITH_KNOTS ( 'NONE', 3,
 ( #6931, #991, #9191, #10178, #8995, #7922, #45, #1993, #11102, #3922, #7996, #12056, #7131, #2907, #12262, #6065, #6992, #4985, #4052, #10118, #9120, #4121, #11056, #11186, #1927, #930, #12192, #5998, #2053, #6123, #1055, #8201, #3111, #7188, #11254, #2117, #9924, #1323, #4184, #11323, #194, #1388, #5320, #12517, #388, #6267, #4251, #1195, #5451, #133, #2186, #6328, #11592, #3439, #12325, #11455, #10519, #4440, #4382, #12457, #10452, #3177, #2312, #3310, #6194, #3370, #7519, #7388, #7453, #6395, #8264, #7258, #10248, #10316, #12583, #9457, #10378, #257, #8331, #1124, #8524, #8463, #5389, #5251, #9322, #12389, #11528, #5181, #3243, #9260, #7325, #11394, #2254, #1256, #2383, #9513, #329 ),
 .UNSPECIFIED., .F., .F.,
 ( 4, 1, 1, 2, 2, 2, 1, 1, 1, 2, 2, 2, 2, 1, 1, 1, 2, 2, 2, 1, 1, 1, 2, 2, 2, 1, 1, 1, 1, 2, 2, 2, 1, 1, 1, 2, 2, 1, 1, 1, 1, 2, 2, 2, 2, 1, 1, 1, 2, 2, 2, 2, 1, 1, 1, 2, 2, 2, 1, 1, 1, 2, 2, 4 ),
 ( 0.000000000000000000, 0.03124999999996640881, 0.04687499999994677174, 0.05468749999993696015, 0.06249999999992715549, 0.09374999999987633503, 0.1093749999998509387, 0.1171874999998381989, 0.1210937499998318428, 0.1230468749998313432, 0.1249999999998308575, 0.1874999999996515565, 0.2187499999995618505, 0.2343749999995169975, 0.2421874999994945710, 0.2460937499994810540, 0.2480468749994765854, 0.2499999999994720890, 0.2812499999993741118, 0.2968749999993226529, 0.3046874999992970623, 0.3085937499992819633, 0.3105468749992766342, 0.3124999999992712496, 0.3437499999991869837, 0.3593749999991447397, 0.3671874999991236455, 0.3710937499991131538, 0.3730468749991098232, 0.3740234374991061039, 0.3749999999991024402, 0.4062499999991214250, 0.4218749999991309729, 0.4296874999991357469, 0.4335937499991380784, 0.4355468749991411870, 0.4374999999991442956, 0.4687499999992265631, 0.4843749999992656985, 0.4921874999992851829, 0.4960937499992930100, 0.4980468749992968958, 0.4999999999993007815, 0.5624999999994121369, 0.5937499999994678701, 0.6093749999994938493, 0.6171874999995067279, 0.6210937499995131672, 0.6230468749995142774, 0.6249999999995153876, 0.6874999999995312638, 0.7187499999995392574, 0.7343749999995432542, 0.7421874999995468070, 0.7460937499995484723, 0.7480468749995492495, 0.7499999999995500266, 0.8124999999996305178, 0.8437499999996695976, 0.8593749999996903588, 0.8671874999997019051, 0.8710937499997087885, 0.8749999999997156719, 1.000000000000000000 ),
 .UNSPECIFIED. ) ;
#694 = ORIENTED_EDGE ( 'NONE', *, *, #9006, .T. ) ;
#695 = EDGE_LOOP ( 'NONE', ( #12036, #7828, #9009, #10772 ) ) ;
#696 = AXIS2_PLACEMENT_3D ( 'NONE', #9666, #11747, #10546 ) ;
#697 = CARTESIAN_POINT ( 'NONE',  ( 8.526617657838038156, 20.08915143297736705, 260.5542428351132571 ) ) ;
#698 = ORIENTED_EDGE ( 'NONE', *, *, #11298, .T. ) ;
#699 = PRODUCT_DEFINITION_SHAPE ( 'NONE', 'NONE',  #13151 ) ;
#700 = AXIS2_PLACEMENT_3D ( 'NONE', #1617, #9734, #9880 ) ;
#701 = DIRECTION ( 'NONE',  ( 0.000000000000000000, 0.000000000000000000, -1.000000000000000000 ) ) ;
#702 = ADVANCED_FACE ( 'NONE', ( #4135 ), #8217, .F. ) ;
#703 = CARTESIAN_POINT ( 'NONE',  ( -239.6752751780965411, 1.974315850608226564, -11.58364238450999828 ) ) ;
#704 = VECTOR ( 'NONE', #243, 1000.000000000000114 ) ;
#705 = CARTESIAN_POINT ( 'NONE',  ( -260.5542428355875018, 20.08915143288246696, -17.05314194217034895 ) ) ;
#706 = LINE ( 'NONE', #8639, #7975 ) ;
#707 =( LENGTH_UNIT ( ) NAMED_UNIT ( * ) SI_UNIT ( .MILLI., .METRE. ) );
#708 = EDGE_CURVE ( 'NONE', #3236, #5526, #10611, .T. ) ;
#709 = ORIENTED_EDGE ( 'NONE', *, *, #6978, .T. ) ;
#710 = CARTESIAN_POINT ( 'NONE',  ( -27.68945685411286561, -19.00000000000000000, 290.6841825403027997 ) ) ;
#711 = VECTOR ( 'NONE', #2929, 1000.000000000000000 ) ;
#712 = ORIENTED_EDGE ( 'NONE', *, *, #12259, .T. ) ;
#713 = STYLED_ITEM ( 'NONE', ( #5636 ), #10422 ) ;
#714 = CARTESIAN_POINT ( 'NONE',  ( -243.2974363841306342, 7.571041528465444870, -8.986772684112915854 ) ) ;
#715 = ORIENTED_EDGE ( 'NONE', *, *, #5260, .T. ) ;
#716 = CLOSED_SHELL ( 'NONE', ( #9981, #4280, #9611, #8563, #12138, #8414, #2407, #1922, #2600, #9168, #537, #7337, #9303, #5842 ) ) ;
#717 = CARTESIAN_POINT ( 'NONE',  ( 0.000000000000000000, -9.830508068699650437, 0.000000000000000000 ) ) ;
#718 = CARTESIAN_POINT ( 'NONE',  ( 31.82909658243173467, -30.00000000000000000, -285.6728570749450569 ) ) ;
#719 = FACE_OUTER_BOUND ( 'NONE', #9816, .T. ) ;
#720 = AXIS2_PLACEMENT_3D ( 'NONE', #12565, #1304, #3418 ) ;
#721 = CARTESIAN_POINT ( 'NONE',  ( -229.8304973814411198, 7.772590954318897793, -8.845180372341092223 ) ) ;
#722 = FACE_BOUND ( 'NONE', #905, .T. ) ;
#723 = CARTESIAN_POINT ( 'NONE',  ( -244.1910629296142474, -8.248580890786996633, 8.715491051944391998 ) ) ;
#724 = CARTESIAN_POINT ( 'NONE',  ( -59.24444182677445525, 20.79694577634646180, -254.0989678903617914 ) ) ;
#725 = CONTEXT_DEPENDENT_SHAPE_REPRESENTATION ( #12551, #7460 ) ;
#726 =( REPRESENTATION_RELATIONSHIP ('NONE','NONE', #12019, #182 ) REPRESENTATION_RELATIONSHIP_WITH_TRANSFORMATION ( #1882 )SHAPE_REPRESENTATION_RELATIONSHIP( ) );
#727 = ORIENTED_EDGE ( 'NONE', *, *, #5095, .T. ) ;
#728 = CARTESIAN_POINT ( 'NONE',  ( -229.7633312047737491, 5.934404468281496037, 10.43166704019080093 ) ) ;
#729 = ORIENTED_EDGE ( 'NONE', *, *, #2530, .F. ) ;
#730 = PRODUCT_DEFINITION_SHAPE ( 'NONE', 'NONE',  #13059 ) ;
#731 = AXIS2_PLACEMENT_3D ( 'NONE', #10333, #9339, #1339 ) ;
#732 = CARTESIAN_POINT ( 'NONE',  ( -249.5790707039662948, -10.95560708710130271, -4.250203459824828833 ) ) ;
#733 = ORIENTED_EDGE ( 'NONE', *, *, #1557, .F. ) ;
#734 = CIRCLE ( 'NONE', #3057, 245.7999999999999829 ) ;
#735 = CARTESIAN_POINT ( 'NONE',  ( -234.8993005735983104, 20.55460285152947009, -115.8123742918138248 ) ) ;
#736 = FACE_OUTER_BOUND ( 'NONE', #11166, .T. ) ;
#737 = CARTESIAN_POINT ( 'NONE',  ( 0.000000000000000000, -9.830508068699650437, 248.1666666666509968 ) ) ;
#738 = EDGE_CURVE ( 'NONE', #6913, #10427, #2201, .T. ) ;
#739 = CARTESIAN_POINT ( 'NONE',  ( -240.1208361041844910, 2.772967769358974710, 11.41810622433049893 ) ) ;
#740 = CARTESIAN_POINT ( 'NONE',  ( -241.5877467168933492, 5.754636832785866574, 10.53299718340092817 ) ) ;
#741 = AXIS2_PLACEMENT_3D ( 'NONE', #10234, #5164, #9243 ) ;
#742 = CARTESIAN_POINT ( 'NONE',  ( 71.82423009839129691, 30.00000000000000000, 202.4354503650404808 ) ) ;
#743 = CARTESIAN_POINT ( 'NONE',  ( 17.68709912901550041, -138.4705547276867321, -37.93010648591155842 ) ) ;
#744 = CARTESIAN_POINT ( 'NONE',  ( 230.0000029335025147, 3.500192773088487641, 0.2278275254128714344 ) ) ;
#745 = ITEM_DEFINED_TRANSFORMATION ( 'NONE', 'NONE', #4266,  #805 ) ;
#746 = CARTESIAN_POINT ( 'NONE',  ( -249.7834965322842322, 11.60135170607461319, 1.863160430829968517 ) ) ;
#747 = DIRECTION ( 'NONE',  ( 0.5469441386039890496, 0.000000000000000000, -0.8371691043312220470 ) ) ;
#748 = CARTESIAN_POINT ( 'NONE',  ( -229.9997816294760753, -11.99584946919181405, 0.3676194914965865146 ) ) ;
#749 = ORIENTED_EDGE ( 'NONE', *, *, #1670, .T. ) ;
#750 = ORIENTED_EDGE ( 'NONE', *, *, #4772, .F. ) ;
#751 = CIRCLE ( 'NONE', #9895, 4.500000000000000000 ) ;
#752 = CARTESIAN_POINT ( 'NONE',  ( -0.000000000000000000, -21.50000000000000000, 0.000000000000000000 ) ) ;
#753 = CARTESIAN_POINT ( 'NONE',  ( -0.000000000000000000, -18.00000000000000000, 0.000000000000000000 ) ) ;
#754 = ADVANCED_FACE ( 'NONE', ( #2461 ), #10175, .T. ) ;
#755 = EDGE_CURVE ( 'NONE', #10156, #9288, #11337, .T. ) ;
#756 = CARTESIAN_POINT ( 'NONE',  ( 84.20717312394452847, 20.55460285104429019, 247.9906035367661161 ) ) ;
#757 = CARTESIAN_POINT ( 'NONE',  ( 0.000000000000000000, 20.00000000000000000, 0.000000000000000000 ) ) ;
#758 = DIRECTION ( 'NONE',  ( 0.9848077530122097967, 0.000000000000000000, -0.1736481776669207000 ) ) ;
#759 = CYLINDRICAL_SURFACE ( 'NONE', #5399, 5.499999999999998224 ) ;
#760 = CARTESIAN_POINT ( 'NONE',  ( 240.1689872792136384, 2.295088600363839770, -2.642490611638467879 ) ) ;
#761 = COLOUR_RGB ( '', 0.72549020, 0.75294118, 0.79215686) ;
#762 = EDGE_LOOP ( 'NONE', ( #5995, #10511, #5433, #10109 ) ) ;
#763 = EDGE_CURVE ( 'NONE', #157, #9833, #7746, .T. ) ;
#764 = CARTESIAN_POINT ( 'NONE',  ( 24.18668477630849267, -19.00000000000000000, -294.9245348571437262 ) ) ;
#765 = ORIENTED_EDGE ( 'NONE', *, *, #8990, .F. ) ;
#766 = ORIENTED_EDGE ( 'NONE', *, *, #2370, .F. ) ;
#767 = CARTESIAN_POINT ( 'NONE',  ( -181.8257142206830679, -30.00000000000000000, -220.1128339014753692 ) ) ;
#768 = ORIENTED_EDGE ( 'NONE', *, *, #6579, .T. ) ;
#769 = CARTESIAN_POINT ( 'NONE',  ( 235.4000000000000057, 0.000000000000000000, 0.000000000000000000 ) ) ;
#770 = CARTESIAN_POINT ( 'NONE',  ( -207.1687172315079692, 20.08915143295307004, 158.9353507253535156 ) ) ;
#771 = DIRECTION ( 'NONE',  ( 0.000000000000000000, 0.7071067811865480168, 0.7071067811865470176 ) ) ;
#772 = CARTESIAN_POINT ( 'NONE',  ( -247.3964713742791446, 9.678883351029913484, 6.661754107376391509 ) ) ;
#773 = ORIENTED_EDGE ( 'NONE', *, *, #9622, .T. ) ;
#774 = DIRECTION ( 'NONE',  ( 0.000000000000000000, 0.000000000000000000, -1.000000000000000000 ) ) ;
#775 = EDGE_CURVE ( 'NONE', #4133, #3138, #10532, .T. ) ;
#776 = ORIENTED_EDGE ( 'NONE', *, *, #6811, .T. ) ;
#777 = ADVANCED_FACE ( 'NONE', ( #6476 ), #6340, .T. ) ;
#778 = CARTESIAN_POINT ( 'NONE',  ( -238.7109915794538892, 0.3295697628469637097, 11.74999996399578350 ) ) ;
#779 = VERTEX_POINT ( 'NONE', #9336 ) ;
#780 = FACE_BOUND ( 'NONE', #6237, .T. ) ;
#781 = DIRECTION ( 'NONE',  ( 0.000000000000000000, 1.000000000000000000, 0.000000000000000000 ) ) ;
#782 = FACE_OUTER_BOUND ( 'NONE', #10358, .T. ) ;
#783 = FACE_BOUND ( 'NONE', #7105, .T. ) ;
#784 = CARTESIAN_POINT ( 'NONE',  ( -245.5461639313266744, -9.015782184408621447, 7.919169856991794099 ) ) ;
#785 = CARTESIAN_POINT ( 'NONE',  ( -107.6783259591024944, 20.79694577634646535, -237.6585102388689279 ) ) ;
#786 = ITEM_DEFINED_TRANSFORMATION ( 'NONE', 'NONE', #6135,  #805 ) ;
#787 = ORIENTED_EDGE ( 'NONE', *, *, #3681, .T. ) ;
#788 = LINE ( 'NONE', #6925, #4779 ) ;
#789 = VERTEX_POINT ( 'NONE', #6537 ) ;
#790 = EDGE_CURVE ( 'NONE', #1462, #3155, #6053, .T. ) ;
#791 = CIRCLE ( 'NONE', #9309, 254.0000000000000000 ) ;
#792 = CARTESIAN_POINT ( 'NONE',  ( -248.3468897632307062, -9.892776367366600709, -6.340645126513342333 ) ) ;
#793 = ORIENTED_EDGE ( 'NONE', *, *, #10673, .F. ) ;
#794 = CARTESIAN_POINT ( 'NONE',  ( 115.8123742916068295, 20.55460285108873819, 234.8993005735927966 ) ) ;
#795 = FACE_OUTER_BOUND ( 'NONE', #836, .T. ) ;
#796 = CARTESIAN_POINT ( 'NONE',  ( 122.2593324768334071, 18.00000000000000000, -174.7755348299895104 ) ) ;
#797 = PRODUCT_DEFINITION_SHAPE ( 'NONE', 'NONE',  #13171 ) ;
#798 = FACE_OUTER_BOUND ( 'NONE', #12920, .T. ) ;
#799 = CIRCLE ( 'NONE', #8038, 5.499999999999998224 ) ;
#800 = CARTESIAN_POINT ( 'NONE',  ( 2.400307726328812375E-14, 30.00000000000000000, -196.0000000000000000 ) ) ;
#801 = DIRECTION ( 'NONE',  ( -0.9659258262890663138, 0.000000000000000000, -0.2588190451025280669 ) ) ;
#802 = CARTESIAN_POINT ( 'NONE',  ( 2.822810872034648951E-14, -19.00000000000000000, 230.0000000000000000 ) ) ;
#803 = PRODUCT_DEFINITION_SHAPE ( 'NONE', 'NONE',  #13111 ) ;
#804 = CARTESIAN_POINT ( 'NONE',  ( -249.7894049735008650, 11.64306034551006164, 1.598052593220072648 ) ) ;
#805 = AXIS2_PLACEMENT_3D ( 'NONE', #6711, #10765, #10635 ) ;
#806 = CARTESIAN_POINT ( 'NONE',  ( -229.9857581487122218, -11.72407015423622489, -2.585718574142970017 ) ) ;
#807 = ORIENTED_EDGE ( 'NONE', *, *, #8174, .F. ) ;
#808 = VERTEX_POINT ( 'NONE', #10590 ) ;
#809 = CARTESIAN_POINT ( 'NONE',  ( 226.7234983661818717, 3.822755691033211001, -0.07535703595917098152 ) ) ;
#810 = DIRECTION ( 'NONE',  ( -1.000000000000000000, 0.000000000000000000, 0.000000000000000000 ) ) ;
#811 = CARTESIAN_POINT ( 'NONE',  ( 234.3927740976959910, 20.79694577647348908, -115.5625104414818054 ) ) ;
#812 = DIRECTION ( 'NONE',  ( 0.000000000000000000, 0.000000000000000000, 1.000000000000000000 ) ) ;
#813 = CARTESIAN_POINT ( 'NONE',  ( 0.000000000000000000, 0.000000000000000000, 0.000000000000000000 ) ) ;
#814 = DIRECTION ( 'NONE',  ( -0.000000000000000000, -1.000000000000000000, 0.000000000000000000 ) ) ;
#815 = ORIENTED_EDGE ( 'NONE', *, *, #7409, .F. ) ;
#816 = EDGE_CURVE ( 'NONE', #2672, #10498, #2429, .T. ) ;
#817 = FACE_BOUND ( 'NONE', #8599, .T. ) ;
#818 = ADVANCED_FACE ( 'NONE', ( #7398, #11406 ), #2262, .F. ) ;
#819 = CIRCLE ( 'NONE', #1885, 248.7999999999999829 ) ;
#820 = CARTESIAN_POINT ( 'NONE',  ( -239.4731782950807712, -1.801843764861105646, 11.86393663232041540 ) ) ;
#821 = EDGE_LOOP ( 'NONE', ( #12068, #9534, #10619, #12082 ) ) ;
#822 = CIRCLE ( 'NONE', #397, 6.500000000000005329 ) ;
#823 = VERTEX_POINT ( 'NONE', #2331 ) ;
#824 = AXIS2_PLACEMENT_3D ( 'NONE', #9221, #9423, #2082 ) ;
#825 = AXIS2_PLACEMENT_3D ( 'NONE', #4397, #12475, #6347 ) ;
#826 = FACE_OUTER_BOUND ( 'NONE', #9682, .T. ) ;
#827 = ORIENTED_EDGE ( 'NONE', *, *, #946, .T. ) ;
#828 = AXIS2_PLACEMENT_3D ( 'NONE', #12222, #3075, #11213 ) ;
#829 =( REPRESENTATION_RELATIONSHIP ('NONE','NONE', #12019, #5191 ) REPRESENTATION_RELATIONSHIP_WITH_TRANSFORMATION ( #10736 )SHAPE_REPRESENTATION_RELATIONSHIP( ) );
#830 = DIRECTION ( 'NONE',  ( 0.6368676505102708330, 0.000000000000000000, 0.7709731485165535192 ) ) ;
#831 = DIRECTION ( 'NONE',  ( -0.8371691043312220470, 0.000000000000000000, -0.5469441386039890496 ) ) ;
#832 = CARTESIAN_POINT ( 'NONE',  ( -239.0397834240491477, -1.254461513564051556, -11.93425063537890374 ) ) ;
#833 = CARTESIAN_POINT ( 'NONE',  ( 0.000000000000000000, 20.00000000000000000, 0.000000000000000000 ) ) ;
#834 = B_SPLINE_CURVE_WITH_KNOTS ( 'NONE', 3,
 ( #11246, #10244, #7057, #12188, #6062, #1121, #130, #4179, #2307, #3365, #2617, #7449, #4379, #10375, #11523, #5386, #386, #12513, #10516, #1386, #2380, #2250, #4680, #8826, #6455, #8521, #5449, #4436, #8392, #9511, #6389, #10449, #9386, #9454, #6704, #12581, #326, #2676, #6765, #3435, #8460, #7517, #1693, #11766, #1319, #5690, #12454, #7321, #10756, #5761, #1624, #3687, #9743, #630, #8757, #12820, #7384, #10819, #3306, #7758, #4749, #11833, #1249, #9819, #697, #12889 ),
 .UNSPECIFIED., .F., .F.,
 ( 4, 2, 2, 2, 2, 2, 2, 2, 2, 2, 2, 2, 2, 2, 2, 2, 2, 2, 2, 2, 2, 2, 2, 2, 2, 2, 2, 2, 2, 2, 2, 2, 4 ),
 ( 0.5000000000000000000, 0.5156250000000000000, 0.5312499999999998890, 0.5468749999999998890, 0.5624999999999998890, 0.5781249999999997780, 0.5937499999999997780, 0.6093749999999997780, 0.6249999999999997780, 0.6406249999999997780, 0.6562499999999997780, 0.6718749999999997780, 0.6874999999999997780, 0.7031249999999997780, 0.7187499999999997780, 0.7343749999999996669, 0.7499999999999997780, 0.7656249999999997780, 0.7812499999999997780, 0.7968749999999997780, 0.8124999999999997780, 0.8281249999999997780, 0.8437499999999997780, 0.8593749999999997780, 0.8749999999999997780, 0.8906249999999998890, 0.9062499999999998890, 0.9218749999999998890, 0.9375000000000000000, 0.9531250000000000000, 0.9687500000000000000, 0.9843750000000000000, 1.000000000000000000 ),
 .UNSPECIFIED. ) ;
#835 = CIRCLE ( 'NONE', #6157, 248.1666666666679930 ) ;
#836 = EDGE_LOOP ( 'NONE', ( #6634, #7940, #7084, #12038 ) ) ;
#837 = FACE_OUTER_BOUND ( 'NONE', #10019, .T. ) ;
#838 = ORIENTED_EDGE ( 'NONE', *, *, #13038, .T. ) ;
#839 = AXIS2_PLACEMENT_3D ( 'NONE', #4366, #3158, #8314 ) ;
#840 = CARTESIAN_POINT ( 'NONE',  ( -239.1986675888292382, 1.476433811303769383, 11.65687006326614039 ) ) ;
#841 = ORIENTED_EDGE ( 'NONE', *, *, #4349, .T. ) ;
#842 = CONICAL_SURFACE ( 'NONE', #2113, 3.823498366181860231, 0.7853981633974476129 ) ;
#843 = CARTESIAN_POINT ( 'NONE',  ( 240.3318468624802620, -2.620158398456138737, -2.323190430600380108 ) ) ;
#844 = CARTESIAN_POINT ( 'NONE',  ( 0.000000000000000000, -19.00000000000000000, 0.000000000000000000 ) ) ;
#845 = CARTESIAN_POINT ( 'NONE',  ( 0.000000000000000000, 21.50000000000000000, 0.000000000000000000 ) ) ;
#846 = EDGE_CURVE ( 'NONE', #5331, #11051, #9586, .T. ) ;
#847 = CARTESIAN_POINT ( 'NONE',  ( -229.6996680450365886, 0.7763087779090785956, -11.75000000000000178 ) ) ;
#848 = ADVANCED_FACE ( 'NONE', ( #5333, #3189 ), #270, .F. ) ;
#849 = DIRECTION ( 'NONE',  ( 0.000000000000000000, -1.000000000000000000, 0.000000000000000000 ) ) ;
#850 = CARTESIAN_POINT ( 'NONE',  ( -241.6809225226833462, -5.875971056079142052, 10.46353150752503502 ) ) ;
#851 = CARTESIAN_POINT ( 'NONE',  ( -238.8090076341308361, 0.7315829127600046444, -11.97771329458992717 ) ) ;
#852 = ITEM_DEFINED_TRANSFORMATION ( 'NONE', 'NONE', #11668,  #805 ) ;
#853 = ORIENTED_EDGE ( 'NONE', *, *, #7856, .T. ) ;
#854 = CARTESIAN_POINT ( 'NONE',  ( -238.7109915777963636, -0.006372640623321836582, -11.74999999916455984 ) ) ;
#855 = CONICAL_SURFACE ( 'NONE', #12555, 6.500000000000005329, 0.7853981633974476129 ) ;
#856 = ORIENTED_EDGE ( 'NONE', *, *, #12058, .F. ) ;
#857 = ORIENTED_EDGE ( 'NONE', *, *, #9638, .T. ) ;
#858 = CARTESIAN_POINT ( 'NONE',  ( -249.2136238162158577, -10.44210856422258082, -5.387711592263697113 ) ) ;
#859 = ORIENTED_EDGE ( 'NONE', *, *, #3793, .F. ) ;
#860 = CARTESIAN_POINT ( 'NONE',  ( -259.6535381480032356, 20.55460285108499008, 34.20858920320377905 ) ) ;
#861 = LINE ( 'NONE', #4921, #12650 ) ;
#862 = CARTESIAN_POINT ( 'NONE',  ( -0.000000000000000000, -29.00000000000000000, 0.000000000000000000 ) ) ;
#863 = PLANE ( 'NONE',  #11658 ) ;
#864 = EDGE_CURVE ( 'NONE', #6987, #11199, #7273, .T. ) ;
#865 = CARTESIAN_POINT ( 'NONE',  ( -246.4289107141176771, 9.384359667912798741, 7.479355994788029705 ) ) ;
#866 = AXIS2_PLACEMENT_3D ( 'NONE', #6070, #9267, #9195 ) ;
#867 =( LENGTH_UNIT ( ) NAMED_UNIT ( * ) SI_UNIT ( .MILLI., .METRE. ) );
#868 = DIRECTION ( 'NONE',  ( 0.1445786100688158937, 0.5538822189107471816, -0.8199460427888388692 ) ) ;
#869 = CARTESIAN_POINT ( 'NONE',  ( -229.9163789481184494, -9.982432720316847252, 6.209677335868705406 ) ) ;
#870 = EDGE_CURVE ( 'NONE', #678, #3753, #734, .T. ) ;
#871 = CONTEXT_DEPENDENT_SHAPE_REPRESENTATION ( #6962, #9721 ) ;
#872 = DIRECTION ( 'NONE',  ( 0.000000000000000000, -1.000000000000000000, 0.000000000000000000 ) ) ;
#873 = ORIENTED_EDGE ( 'NONE', *, *, #8104, .T. ) ;
#874 = ORIENTED_EDGE ( 'NONE', *, *, #3863, .F. ) ;
#875 = CONTEXT_DEPENDENT_SHAPE_REPRESENTATION ( #7964, #4757 ) ;
#876 = DIRECTION ( 'NONE',  ( 0.000000000000000000, 0.9998057603070481525, -0.01970892327970900221 ) ) ;
#877 = CARTESIAN_POINT ( 'NONE',  ( -290.6841825403030839, -18.00000000000000000, -27.68945685411394919 ) ) ;
#878 = FACE_OUTER_BOUND ( 'NONE', #3268, .T. ) ;
#879 = CIRCLE ( 'NONE', #6214, 251.2912898646364397 ) ;
#880 = CARTESIAN_POINT ( 'NONE',  ( 0.000000000000000000, 30.00000000000000000, -208.0000000000000000 ) ) ;
#881 = CARTESIAN_POINT ( 'NONE',  ( 0.000000000000000000, 0.000000000000000000, 0.000000000000000000 ) ) ;
#882 = CARTESIAN_POINT ( 'NONE',  ( -245.3969493176729486, -8.938055201230712399, 7.627167029050283986 ) ) ;
#883 = ITEM_DEFINED_TRANSFORMATION ( 'NONE', 'NONE', #8056,  #805 ) ;
#884 = AXIS2_PLACEMENT_3D ( 'NONE', #12840, #5778, #12647 ) ;
#885 = CARTESIAN_POINT ( 'NONE',  ( -239.4731783641827860, 1.801843830935816015, -11.86393662238275226 ) ) ;
#886 = ORIENTED_EDGE ( 'NONE', *, *, #7689, .F. ) ;
#887 = DIRECTION ( 'NONE',  ( 1.000000000000000000, 0.000000000000000000, 0.000000000000000000 ) ) ;
#888 = CARTESIAN_POINT ( 'NONE',  ( -239.0548353902184431, -1.279873199611678114, 11.93155240848446219 ) ) ;
#889 = VERTEX_POINT ( 'NONE', #7468 ) ;
#890 = ORIENTED_EDGE ( 'NONE', *, *, #10293, .T. ) ;
#891 = DIRECTION ( 'NONE',  ( 0.6368676505102707219, 0.000000000000000000, 0.7709731485165535192 ) ) ;
#892 = DIRECTION ( 'NONE',  ( 0.000000000000000000, -1.000000000000000000, 0.000000000000000000 ) ) ;
#893 = CARTESIAN_POINT ( 'NONE',  ( 160.6180214586902366, 11.79660968244693997, 194.4394280558747994 ) ) ;
#894 = AXIS2_PLACEMENT_3D ( 'NONE', #1605, #600, #9791 ) ;
#895 = EDGE_CURVE ( 'NONE', #6702, #6924, #4337, .T. ) ;
#896 = CARTESIAN_POINT ( 'NONE',  ( -247.8175805188620018, 19.96883746128897386, -84.14846197934974725 ) ) ;
#897 = DIRECTION ( 'NONE',  ( 0.000000000000000000, 0.000000000000000000, 1.000000000000000000 ) ) ;
#898 = CARTESIAN_POINT ( 'NONE',  ( 0.000000000000000000, 0.000000000000000000, 0.000000000000000000 ) ) ;
#899 = CARTESIAN_POINT ( 'NONE',  ( -246.6923348789300974, 9.470909649984781353, 6.954450552248236050 ) ) ;
#900 = VERTEX_POINT ( 'NONE', #8538 ) ;
#901 = DIRECTION ( 'NONE',  ( 0.000000000000000000, 1.000000000000000000, 0.000000000000000000 ) ) ;
#902 = VECTOR ( 'NONE', #1414, 1000.000000000000000 ) ;
#903 = ORIENTED_EDGE ( 'NONE', *, *, #3096, .F. ) ;
#904 = CARTESIAN_POINT ( 'NONE',  ( -245.6300371787731365, 9.052739546773430845, -7.492707602044229809 ) ) ;
#905 = EDGE_LOOP ( 'NONE', ( #12477, #7810 ) ) ;
#906 = VECTOR ( 'NONE', #7554, 1000.000000000000000 ) ;
#907 = AXIS2_PLACEMENT_3D ( 'NONE', #1181, #52, #3230 ) ;
#908 = LINE ( 'NONE', #2961, #1944 ) ;
#909 = DIRECTION ( 'NONE',  ( 0.000000000000000000, 0.000000000000000000, 1.000000000000000000 ) ) ;
#910 = DIRECTION ( 'NONE',  ( 0.6368676505102709440, 0.000000000000000000, 0.7709731485165532971 ) ) ;
#911 = EDGE_CURVE ( 'NONE', #10031, #1416, #5411, .T. ) ;
#912 = DIRECTION ( 'NONE',  ( 0.000000000000000000, -1.000000000000000000, 0.000000000000000000 ) ) ;
#913 = CARTESIAN_POINT ( 'NONE',  ( 0.000000000000000000, 30.00000000000000000, 214.5000000000000000 ) ) ;
#914 = APPLICATION_CONTEXT ( 'automotive_design' ) ;
#915 = PRODUCT_DEFINITION_SHAPE ( 'NONE', 'NONE',  #13100 ) ;
#916 = CARTESIAN_POINT ( 'NONE',  ( -241.3090253319653016, -5.344653766038736542, 10.74405649903519055 ) ) ;
#917 = AXIS2_PLACEMENT_3D ( 'NONE', #6215, #3326, #2401 ) ;
#918 = CARTESIAN_POINT ( 'NONE',  ( -239.1644449882676042, 1.447449306433101768, -11.91236063194371830 ) ) ;
#919 = UNCERTAINTY_MEASURE_WITH_UNIT (LENGTH_MEASURE( 1.000000000000000082E-05 ), #5049, 'distance_accuracy_value', 'NONE');
#920 = ORIENTED_EDGE ( 'NONE', *, *, #11171, .T. ) ;
#921 = CARTESIAN_POINT ( 'NONE',  ( 0.000000000000000000, -2.772967769359314882, 0.000000000000000000 ) ) ;
#922 = ORIENTED_EDGE ( 'NONE', *, *, #9814, .T. ) ;
#923 = ADVANCED_FACE ( 'NONE', ( #5595 ), #11154, .F. ) ;
#924 = ORIENTED_EDGE ( 'NONE', *, *, #10395, .F. ) ;
#925 = CARTESIAN_POINT ( 'NONE',  ( -249.7854625206820174, -11.61528754001802000, 1.774251678600656579 ) ) ;
#926 = VERTEX_POINT ( 'NONE', #12719 ) ;
#927 = VECTOR ( 'NONE', #6570, 1000.000000000000000 ) ;
#928 = CIRCLE ( 'NONE', #6884, 6.500000000000005329 ) ;
#929 = CARTESIAN_POINT ( 'NONE',  ( -1.010328782420808020E-12, 20.79694577634649022, 260.7745447061710138 ) ) ;
#930 = CARTESIAN_POINT ( 'NONE',  ( -246.3126759744927483, 9.340233780095946514, -7.533927936320575114 ) ) ;
#931 = DIRECTION ( 'NONE',  ( 0.6368676505102707219, 0.000000000000000000, 0.7709731485165535192 ) ) ;
#932 = AXIS2_PLACEMENT_3D ( 'NONE', #1531, #10591, #3525 ) ;
#933 = CARTESIAN_POINT ( 'NONE',  ( 0.000000000000000000, 2.156506209390990136, 0.000000000000000000 ) ) ;
#934 = CARTESIAN_POINT ( 'NONE',  ( -243.0176490155954809, 7.336472069124719830, 9.496559185463413044 ) ) ;
#935 = SURFACE_STYLE_USAGE ( .BOTH. , #10063 ) ;
#936 = DIRECTION ( 'NONE',  ( -0.3420201433256601642, 0.000000000000000000, -0.9396926207859115365 ) ) ;
#937 = CARTESIAN_POINT ( 'NONE',  ( -229.7834611933087103, -6.213105212076664330, 9.980295640892103748 ) ) ;
#938 = EDGE_CURVE ( 'NONE', #8755, #4344, #11803, .T. ) ;
#939 = ADVANCED_FACE ( 'NONE', ( #6672 ), #10407, .F. ) ;
#940 = DIRECTION ( 'NONE',  ( 0.000000000000000000, 1.000000000000000000, 0.000000000000000000 ) ) ;
#941 = VERTEX_POINT ( 'NONE', #11733 ) ;
#942 = ORIENTED_EDGE ( 'NONE', *, *, #8746, .F. ) ;
#943 = CARTESIAN_POINT ( 'NONE',  ( 286.5445428119865028, -30.00000000000000000, 22.67813138875427015 ) ) ;
#944 = CARTESIAN_POINT ( 'NONE',  ( -229.6889200636375108, 1.000000000000000000, 11.95826074310140008 ) ) ;
#945 = VECTOR ( 'NONE', #7892, 1000.000000000000000 ) ;
#946 = EDGE_CURVE ( 'NONE', #9833, #6599, #2775, .T. ) ;
#947 = CARTESIAN_POINT ( 'NONE',  ( 122.2593324768334071, 30.00000000000000000, -174.7755348299895104 ) ) ;
#948 = CYLINDRICAL_SURFACE ( 'NONE', #11772, 5.500000000000005329 ) ;
#949 = DIRECTION ( 'NONE',  ( -0.000000000000000000, -1.000000000000000000, 0.000000000000000000 ) ) ;
#950 = DIRECTION ( 'NONE',  ( 0.6427876096865301481, 0.000000000000000000, 0.7660444431189860071 ) ) ;
#951 = CARTESIAN_POINT ( 'NONE',  ( -245.1951802402266196, -8.836085397833034705, 7.745290892887734202 ) ) ;
#952 = ITEM_DEFINED_TRANSFORMATION ( 'NONE', 'NONE', #11678,  #805 ) ;
#953 = VERTEX_POINT ( 'NONE', #595 ) ;
#954 = FACE_OUTER_BOUND ( 'NONE', #7686, .T. ) ;
#955 = AXIS2_PLACEMENT_3D ( 'NONE', #9704, #11726, #9580 ) ;
#956 = EDGE_CURVE ( 'NONE', #1185, #6599, #12116, .T. ) ;
#957 = CARTESIAN_POINT ( 'NONE',  ( -289.8128292627096130, -30.00000000000000000, 10.41748504886635907 ) ) ;
#958 = EDGE_LOOP ( 'NONE', ( #8262, #10296, #3960, #7089 ) ) ;
#959 = ORIENTED_EDGE ( 'NONE', *, *, #1758, .F. ) ;
#960 = CARTESIAN_POINT ( 'NONE',  ( -0.000000000000000000, -11.79660968244695951, 0.000000000000000000 ) ) ;
#961 = ORIENTED_EDGE ( 'NONE', *, *, #1670, .F. ) ;
#962 = CARTESIAN_POINT ( 'NONE',  ( -248.5304950464277454, 9.965644880941075812, 6.224989825353040018 ) ) ;
#963 = CARTESIAN_POINT ( 'NONE',  ( 247.2466869560049929, 20.08915143286045790, 83.95474316005440585 ) ) ;
#964 = CONICAL_SURFACE ( 'NONE', #10965, 3.000000000000000000, 0.7853981633974461696 ) ;
#965 = DIRECTION ( 'NONE',  ( 0.4503334343941555740, 0.7071067811865490160, 0.5451603414287971017 ) ) ;
#966 = CARTESIAN_POINT ( 'NONE',  ( -241.4660365534715822, 5.559932089232387575, 10.35152193433334311 ) ) ;
#967 = EDGE_LOOP ( 'NONE', ( #4621, #2287, #10425, #1560 ) ) ;
#968 = DIRECTION ( 'NONE',  ( -0.000000000000000000, 0.01970892327970912364, 0.9998057603070482635 ) ) ;
#969 = ORIENTED_EDGE ( 'NONE', *, *, #5981, .F. ) ;
#970 = CARTESIAN_POINT ( 'NONE',  ( -238.9359159396491634, 1.030912813916464055, 11.70469087026479826 ) ) ;
#971 = ORIENTED_EDGE ( 'NONE', *, *, #6486, .F. ) ;
#972 = TOROIDAL_SURFACE ( 'NONE', #548, 241.5000000000000000, 2.500000000000000000 ) ;
#973 =( REPRESENTATION_RELATIONSHIP ('NONE','NONE', #12019, #182 ) REPRESENTATION_RELATIONSHIP_WITH_TRANSFORMATION ( #9755 )SHAPE_REPRESENTATION_RELATIONSHIP( ) );
#974 = AXIS2_PLACEMENT_3D ( 'NONE', #10227, #10426, #7369 ) ;
#975 = DIRECTION ( 'NONE',  ( -0.6368676505102707219, 0.000000000000000000, -0.7709731485165535192 ) ) ;
#976 = CARTESIAN_POINT ( 'NONE',  ( 0.000000000000000000, -2.772967769359314882, 0.000000000000000000 ) ) ;
#977 = CARTESIAN_POINT ( 'NONE',  ( 239.1385365879787344, 0.8886010998292401819, 3.385772393335270358 ) ) ;
#978 = DIRECTION ( 'NONE',  ( 0.000000000000000000, 0.9998057603070481525, -0.01970892327970899874 ) ) ;
#979 = FACE_OUTER_BOUND ( 'NONE', #7181, .T. ) ;
#980 = DIRECTION ( 'NONE',  ( -0.000000000000000000, 1.000000000000000000, 0.000000000000000000 ) ) ;
#981 = CARTESIAN_POINT ( 'NONE',  ( -238.8461604313190492, 0.8432863473122946818, -11.97040126065660282 ) ) ;
#982 = VERTEX_POINT ( 'NONE', #9713 ) ;
#983 = PLANE ( 'NONE',  #9235 ) ;
#984 = ORIENTED_EDGE ( 'NONE', *, *, #6119, .T. ) ;
#985 = CARTESIAN_POINT ( 'NONE',  ( -247.9076433805199144, -9.798874666935999400, -6.926911304953004667 ) ) ;
#986 = EDGE_CURVE ( 'NONE', #7844, #5825, #4648, .T. ) ;
#987 = ADVANCED_FACE ( 'NONE', ( #665, #10924 ), #6799, .F. ) ;
#988 = CARTESIAN_POINT ( 'NONE',  ( -249.4432382448479473, -10.72467464912286239, 4.802290507069141512 ) ) ;
#989 = ORIENTED_EDGE ( 'NONE', *, *, #7409, .T. ) ;
#990 = CARTESIAN_POINT ( 'NONE',  ( 34.13493237066314379, 20.79694577651677889, -259.0935598596149703 ) ) ;
#991 = CARTESIAN_POINT ( 'NONE',  ( -249.5626403296618605, 9.995018771278006753, -6.640755139182748401 ) ) ;
#992 = CYLINDRICAL_SURFACE ( 'NONE', #8296, 11.75000000000000000 ) ;
#993 = CARTESIAN_POINT ( 'NONE',  ( -245.4266968893038268, -8.952647108764159256, -7.610034336731980709 ) ) ;
#994 = CARTESIAN_POINT ( 'NONE',  ( -243.3783983494642769, 7.645447681623645408, 9.249237797097162428 ) ) ;
#995 = PRODUCT_RELATED_PRODUCT_CATEGORY ( 'part', '', ( #334 ) ) ;
#996 = SURFACE_STYLE_FILL_AREA ( #11127 ) ;
#997 = CARTESIAN_POINT ( 'NONE',  ( 20.92562098022501615, -138.4705547276867321, 36.24423871768005512 ) ) ;
#998 = FACE_OUTER_BOUND ( 'NONE', #9183, .T. ) ;
#999 = CONTEXT_DEPENDENT_SHAPE_REPRESENTATION ( #10104, #9842 ) ;
#1000 = DIRECTION ( 'NONE',  ( 0.000000000000000000, -0.9998057603070481525, 0.01970892327970883220 ) ) ;
#1001 = VERTEX_POINT ( 'NONE', #9655 ) ;
#1002 = ORIENTED_EDGE ( 'NONE', *, *, #11588, .T. ) ;
#1003 = CARTESIAN_POINT ( 'NONE',  ( -17.09264059776470290, 19.96883746054087538, 261.1558126970361400 ) ) ;
#1004 = LINE ( 'NONE', #4497, #7838 ) ;
#1005 = PLANE ( 'NONE',  #8520 ) ;
#1006 = EDGE_CURVE ( 'NONE', #5643, #171, #9763, .T. ) ;
#1007 = CARTESIAN_POINT ( 'NONE',  ( 207.3438552934050279, 20.79694577613707551, 159.0697709850429931 ) ) ;
#1008 = EDGE_CURVE ( 'NONE', #3488, #5812, #6737, .T. ) ;
#1009 = LINE ( 'NONE', #4940, #1131 ) ;
#1010 = DIRECTION ( 'NONE',  ( 0.08715574274764503748, 0.000000000000000000, 0.9961946980917466554 ) ) ;
#1011 = CARTESIAN_POINT ( 'NONE',  ( 3.073863465859856636E-14, 24.99999999999995737, 251.0000000000000000 ) ) ;
#1012 = ITEM_DEFINED_TRANSFORMATION ( 'NONE', 'NONE', #6990,  #805 ) ;
#1013 = CIRCLE ( 'NONE', #2494, 2.475000000000000089 ) ;
#1014 = EDGE_LOOP ( 'NONE', ( #2566, #12900, #7199, #5656 ) ) ;
#1015 = DIRECTION ( 'NONE',  ( 1.224646799147349509E-16, 0.000000000000000000, -1.000000000000000000 ) ) ;
#1016 = CARTESIAN_POINT ( 'NONE',  ( 229.9799723853240039, -1.753250733347112345, 3.037834540539402717 ) ) ;
#1017 = VERTEX_POINT ( 'NONE', #7790 ) ;
#1018 = ORIENTED_EDGE ( 'NONE', *, *, #10942, .F. ) ;
#1019 = DIRECTION ( 'NONE',  ( 0.6368676505102707219, 0.000000000000000000, 0.7709731485165535192 ) ) ;
#1020 = VERTEX_POINT ( 'NONE', #10729 ) ;
#1021 = PRODUCT_DEFINITION_SHAPE ( 'NONE', 'NONE',  #13102 ) ;
#1022 = CARTESIAN_POINT ( 'NONE',  ( 196.2980642840460064, 20.08915143284461280, 172.1812796681624889 ) ) ;
#1023 = EDGE_CURVE ( 'NONE', #11697, #2079, #4230, .T. ) ;
#1024 = CARTESIAN_POINT ( 'NONE',  ( -239.4312206625581609, -1.760784905609661166, -11.87011525670738266 ) ) ;
#1025 = CARTESIAN_POINT ( 'NONE',  ( 0.000000000000000000, 0.000000000000000000, 0.000000000000000000 ) ) ;
#1026 = CARTESIAN_POINT ( 'NONE',  ( -246.7886136405148818, 9.502664448782068618, 6.911022175809039325 ) ) ;
#1027 = ORIENTED_EDGE ( 'NONE', *, *, #1507, .T. ) ;
#1028 = CARTESIAN_POINT ( 'NONE',  ( 254.0989678903617346, 20.79694577634646890, 59.24444182677502369 ) ) ;
#1029 = TOROIDAL_SURFACE ( 'NONE', #4427, 252.1999999999999886, 2.000000000000000000 ) ;
#1030 = EDGE_CURVE ( 'NONE', #3384, #7222, #197, .T. ) ;
#1031 = TOROIDAL_SURFACE ( 'NONE', #11888, 238.4705882352940307, 2.000000000000000000 ) ;
#1033 = ORIENTED_EDGE ( 'NONE', *, *, #11937, .T. ) ;
#1032 = AXIS2_PLACEMENT_3D ( 'NONE', #4738, #12020, #7948 ) ;
#1034 = CARTESIAN_POINT ( 'NONE',  ( -245.3907676186766764, 8.935007734144498670, -7.630737089751100655 ) ) ;
#1035 = EDGE_LOOP ( 'NONE', ( #566, #11162, #7813, #5039 ) ) ;
#1036 = CARTESIAN_POINT ( 'NONE',  ( 3.059167704270088292E-14, -19.00000000000000000, -249.7999999999999545 ) ) ;
#1037 = SURFACE_STYLE_FILL_AREA ( #1733 ) ;
#1038 = CARTESIAN_POINT ( 'NONE',  ( 239.3703217814042716, 1.345486616892404230, 3.231439195586080171 ) ) ;
#1039 = CARTESIAN_POINT ( 'NONE',  ( 235.4000000000000057, -2.999417280921144346, 0.05912676983912699968 ) ) ;
#1040 = AXIS2_PLACEMENT_3D ( 'NONE', #2332, #3322, #7399 ) ;
#1041 = CARTESIAN_POINT ( 'NONE',  ( -221.3800702329286594, 20.08915143297736705, -137.6665579279355711 ) ) ;
#1042 = CARTESIAN_POINT ( 'NONE',  ( 0.000000000000000000, -20.00000000000000000, 0.000000000000000000 ) ) ;
#1043 = VECTOR ( 'NONE', #4814, 1000.000000000000000 ) ;
#1044 = CARTESIAN_POINT ( 'NONE',  ( -237.6585102388685584, 20.79694577634646535, -107.6783259591029918 ) ) ;
#1045 = VERTEX_POINT ( 'NONE', #7723 ) ;
#1046 = CARTESIAN_POINT ( 'NONE',  ( -239.2239471121744998, -1.510219381902923264, -11.65254212220749075 ) ) ;
#1047 = CIRCLE ( 'NONE', #6376, 251.1999999999999886 ) ;
#1048 = ORIENTED_EDGE ( 'NONE', *, *, #200, .T. ) ;
#1049 = CARTESIAN_POINT ( 'NONE',  ( -249.3105109839077045, 10.55009524027425982, -5.172972615342095182 ) ) ;
#1050 = CARTESIAN_POINT ( 'NONE',  ( -249.1334134305279804, -9.986442412942713176, -6.653676027923776104 ) ) ;
#1051 = VECTOR ( 'NONE', #5097, 1000.000000000000114 ) ;
#1052 = CARTESIAN_POINT ( 'NONE',  ( -249.7763361841028882, -11.55065150920177075, 2.186104016062915711 ) ) ;
#1053 = ORIENTED_EDGE ( 'NONE', *, *, #543, .T. ) ;
#1054 = CARTESIAN_POINT ( 'NONE',  ( 172.3268284095375122, 20.79694577629726027, -196.4640694357605071 ) ) ;
#1055 = CARTESIAN_POINT ( 'NONE',  ( -245.7661201680033116, 9.116795905909876652, -7.802929255001362030 ) ) ;
#1056 = VECTOR ( 'NONE', #2935, 1000.000000000000114 ) ;
#1057 = DIRECTION ( 'NONE',  ( 0.000000000000000000, 1.000000000000000000, 0.000000000000000000 ) ) ;
#1058 = CARTESIAN_POINT ( 'NONE',  ( -245.0777337248563299, -8.776737537879517603, -7.814324104198428600 ) ) ;
#1059 = CARTESIAN_POINT ( 'NONE',  ( -246.9756885468848964, 9.564884955133036826, 7.246373649300591246 ) ) ;
#1060 = ADVANCED_FACE ( 'NONE', ( #3783 ), #3590, .F. ) ;
#1061 = CIRCLE ( 'NONE', #12129, 5.100000000000003197 ) ;
#1062 = DIRECTION ( 'NONE',  ( 0.7210484489137231057, 0.5538822189107471816, -0.4162975160790912121 ) ) ;
#1063 = CARTESIAN_POINT ( 'NONE',  ( -229.9700272232702503, -11.15178693234673801, 3.780588754129759810 ) ) ;
#1064 = AXIS2_PLACEMENT_3D ( 'NONE', #9512, #12706, #3569 ) ;
#1065 = FACE_OUTER_BOUND ( 'NONE', #4750, .T. ) ;
#1066 = ORIENTED_EDGE ( 'NONE', *, *, #7505, .F. ) ;
#1067 = ORIENTED_EDGE ( 'NONE', *, *, #11182, .T. ) ;
#1068 = CARTESIAN_POINT ( 'NONE',  ( 115.4648407707963997, 20.08915143305429041, -234.1947771728865177 ) ) ;
#1069 = DIRECTION ( 'NONE',  ( 0.000000000000000000, 0.000000000000000000, -1.000000000000000000 ) ) ;
#1070 = CARTESIAN_POINT ( 'NONE',  ( 222.8706404512946904, 3.349349297028606731, -0.06602489298702507448 ) ) ;
#1071 = AXIS2_PLACEMENT_3D ( 'NONE', #3596, #7403, #7664 ) ;
#1072 = DIRECTION ( 'NONE',  ( 0.000000000000000000, 1.000000000000000000, 0.000000000000000000 ) ) ;
#1073 = CARTESIAN_POINT ( 'NONE',  ( 196.4640694362159934, 20.79694577623644491, 172.3268284092819727 ) ) ;
#1074 = EDGE_CURVE ( 'NONE', #5758, #1246, #3524, .T. ) ;
#1075 = CYLINDRICAL_SURFACE ( 'NONE', #11982, 5.500000000000007994 ) ;
#1076 = DIRECTION ( 'NONE',  ( 0.9961946980917446570, 0.000000000000000000, 0.08715574274766850482 ) ) ;
#1077 = VECTOR ( 'NONE', #1474, 1000.000000000000000 ) ;
#1078 = CARTESIAN_POINT ( 'NONE',  ( -242.9854649072008783, -7.295305384121596681, 9.211094754432867404 ) ) ;
#1079 = ORIENTED_EDGE ( 'NONE', *, *, #1023, .T. ) ;
#1080 = FACE_BOUND ( 'NONE', #12639, .T. ) ;
#1081 = PRODUCT_DEFINITION_FORMATION_WITH_SPECIFIED_SOURCE ( 'ANY', '', #6399, .NOT_KNOWN. ) ;
#1082 = DIRECTION ( 'NONE',  ( 0.000000000000000000, 1.000000000000000000, 0.000000000000000000 ) ) ;
#1083 = EDGE_LOOP ( 'NONE', ( #9380, #8970, #4045, #3801 ) ) ;
#1084 = ORIENTED_EDGE ( 'NONE', *, *, #1420, .T. ) ;
#1085 = EDGE_CURVE ( 'NONE', #5993, #10156, #1895, .T. ) ;
#1086 = ADVANCED_FACE ( 'NONE', ( #736 ), #6375, .F. ) ;
#1087 = CARTESIAN_POINT ( 'NONE',  ( 226.7234983661818717, 0.000000000000000000, 0.000000000000000000 ) ) ;
#1088 = CARTESIAN_POINT ( 'NONE',  ( 122.2593324768346008, 29.00000000000000000, 168.2755348299889988 ) ) ;
#1089 = CARTESIAN_POINT ( 'NONE',  ( -67.71318189764485851, 19.96883746024804651, -252.8031682270704437 ) ) ;
#1090 = CIRCLE ( 'NONE', #4284, 249.7999999999999829 ) ;
#1091 = CIRCLE ( 'NONE', #7432, 5.500000000000005329 ) ;
#1092 = DIRECTION ( 'NONE',  ( 0.6368676505102707219, 0.000000000000000000, 0.7709731485165535192 ) ) ;
#1093 = DIRECTION ( 'NONE',  ( 1.000000000000000000, 0.000000000000000000, 0.000000000000000000 ) ) ;
#1094 = CARTESIAN_POINT ( 'NONE',  ( -243.8684449385701498, 8.017730970305375848, 8.590997659349747906 ) ) ;
#1095 = ORIENTED_EDGE ( 'NONE', *, *, #10168, .F. ) ;
#1096 = DIRECTION ( 'NONE',  ( -0.6368676505102707219, 0.000000000000000000, -0.7709731485165535192 ) ) ;
#1098 = ORIENTED_EDGE ( 'NONE', *, *, #3769, .F. ) ;
#1097 = CIRCLE ( 'NONE', #11097, 250.7029414592220178 ) ;
#1099 = DIRECTION ( 'NONE',  ( 0.000000000000000000, 1.000000000000000000, 0.000000000000000000 ) ) ;
#1100 = VERTEX_POINT ( 'NONE', #2649 ) ;
#1101 = EDGE_CURVE ( 'NONE', #10423, #5861, #4770, .T. ) ;
#1102 = CARTESIAN_POINT ( 'NONE',  ( 225.1241593668336236, -30.00000000000000000, -185.9653539489990521 ) ) ;
#1103 = ADVANCED_FACE ( 'NONE', ( #5357 ), #6495, .F. ) ;
#1104 =( REPRESENTATION_RELATIONSHIP ('NONE','NONE', #12019, #5191 ) REPRESENTATION_RELATIONSHIP_WITH_TRANSFORMATION ( #7716 )SHAPE_REPRESENTATION_RELATIONSHIP( ) );
#1105 = CARTESIAN_POINT ( 'NONE',  ( -0.000000000000000000, -3.165711975795909891E-14, 0.000000000000000000 ) ) ;
#1106 = PRESENTATION_STYLE_ASSIGNMENT (( #4169 ) ) ;
#1107 = DIRECTION ( 'NONE',  ( -0.000000000000000000, -1.000000000000000000, 0.000000000000000000 ) ) ;
#1108 = DIRECTION ( 'NONE',  ( 0.6368676505102716101, 0.000000000000000000, 0.7709731485165527420 ) ) ;
#1109 = ADVANCED_FACE ( 'NONE', ( #9059 ), #7125, .T. ) ;
#1110 = CARTESIAN_POINT ( 'NONE',  ( -83.79436865282308133, 20.08915143297736705, -246.8597181602071373 ) ) ;
#1111 = DIRECTION ( 'NONE',  ( 0.000000000000000000, 1.000000000000000000, 0.000000000000000000 ) ) ;
#1112 = CARTESIAN_POINT ( 'NONE',  ( -221.5672498511017920, 20.79694577634646535, -137.7829567244535269 ) ) ;
#1113 = ITEM_DEFINED_TRANSFORMATION ( 'NONE', 'NONE', #8048,  #805 ) ;
#1114 = ORIENTED_EDGE ( 'NONE', *, *, #42, .T. ) ;
#1115 = DIRECTION ( 'NONE',  ( -0.000000000000000000, -1.000000000000000000, 0.000000000000000000 ) ) ;
#1116 = AXIS2_PLACEMENT_3D ( 'NONE', #8493, #3406, #7418 ) ;
#1117 = EDGE_LOOP ( 'NONE', ( #10369, #10140, #8988, #2393 ) ) ;
#1118 = AXIS2_PLACEMENT_3D ( 'NONE', #1698, #2559, #831 ) ;
#1119 = FACE_OUTER_BOUND ( 'NONE', #12151, .T. ) ;
#1120 = CARTESIAN_POINT ( 'NONE',  ( -243.3783983492338052, -7.645447681435416420, -9.249237797260425609 ) ) ;
#1121 = CARTESIAN_POINT ( 'NONE',  ( 59.19439222780464149, 20.08915143297736350, -253.8843055347118138 ) ) ;
#1122 = ORIENTED_EDGE ( 'NONE', *, *, #12541, .F. ) ;
#1123 = CARTESIAN_POINT ( 'NONE',  ( 159.0697709834164755, 20.79694577659177313, 207.3438552932204857 ) ) ;
#1124 = CARTESIAN_POINT ( 'NONE',  ( -241.4289589285359909, 5.524154699870469365, -10.65313710557074600 ) ) ;
#1125 = CARTESIAN_POINT ( 'NONE',  ( 185.9653539490014111, -19.00000000000000000, 225.1241593668316625 ) ) ;
#1126 = CARTESIAN_POINT ( 'NONE',  ( -242.2132964870661453, -6.511711374284875120, -9.780601349847026782 ) ) ;
#1127 = AXIS2_PLACEMENT_3D ( 'NONE', #9176, #12175, #4106 ) ;
#1128 = CARTESIAN_POINT ( 'NONE',  ( -210.0000000000000000, 28.60000000000000142, 5.100000000000000533 ) ) ;
#1129 = DIRECTION ( 'NONE',  ( 0.8325950321581960800, 0.5538822189107472926, 8.720970052781520574E-15 ) ) ;
#1130 = CARTESIAN_POINT ( 'NONE',  ( -229.7038372623077294, 2.825322550619665307, -11.66863389586242405 ) ) ;
#1131 = VECTOR ( 'NONE', #10947, 1000.000000000000000 ) ;
#1132 = AXIS2_PLACEMENT_3D ( 'NONE', #7511, #5571, #9628 ) ;
#1133 = DIRECTION ( 'NONE',  ( 0.000000000000000000, 1.000000000000000000, 0.000000000000000000 ) ) ;
#1134 = CONICAL_SURFACE ( 'NONE', #2404, 6.499999999999999112, 0.7853981633974476129 ) ;
#1135 = ORIENTED_EDGE ( 'NONE', *, *, #3577, .F. ) ;
#1136 = ORIENTED_EDGE ( 'NONE', *, *, #7872, .T. ) ;
#1137 = ADVANCED_FACE ( 'NONE', ( #5929 ), #1377, .T. ) ;
#1138 = CARTESIAN_POINT ( 'NONE',  ( -130.5770120867059916, 20.08915143302827744, -226.1171533162815024 ) ) ;
#1139 = DIRECTION ( 'NONE',  ( 0.000000000000000000, -0.8757116489157734662, -0.4828344519120573719 ) ) ;
#1140 = AXIS2_PLACEMENT_3D ( 'NONE', #3870, #810, #11684 ) ;
#1141 = LINE ( 'NONE', #5200, #7870 ) ;
#1142 = DIRECTION ( 'NONE',  ( 0.000000000000000000, -1.000000000000000000, 0.000000000000000000 ) ) ;
#1143 = CYLINDRICAL_SURFACE ( 'NONE', #4730, 12.00000000000000000 ) ;
#1144 = VECTOR ( 'NONE', #5770, 1000.000000000000000 ) ;
#1145 = FACE_OUTER_BOUND ( 'NONE', #9493, .T. ) ;
#1146 = CARTESIAN_POINT ( 'NONE',  ( 0.000000000000000000, 0.000000000000000000, 0.000000000000000000 ) ) ;
#1147 = CARTESIAN_POINT ( 'NONE',  ( -242.4218346680387697, -6.744440866289951764, 9.622654848396397398 ) ) ;
#1148 = ITEM_DEFINED_TRANSFORMATION ( 'NONE', 'NONE', #11889,  #805 ) ;
#1149 =( REPRESENTATION_RELATIONSHIP ('NONE','NONE', #12019, #182 ) REPRESENTATION_RELATIONSHIP_WITH_TRANSFORMATION ( #852 )SHAPE_REPRESENTATION_RELATIONSHIP( ) );
#1150 = ORIENTED_EDGE ( 'NONE', *, *, #12559, .F. ) ;
#1151 = CARTESIAN_POINT ( 'NONE',  ( 240.6264023546199553, -3.484414313218967774, 0.3842028182350827881 ) ) ;
#1152 = CARTESIAN_POINT ( 'NONE',  ( 229.9831877374639646, -2.133736550081812844, 2.783791508809775550 ) ) ;
#1153 = EDGE_LOOP ( 'NONE', ( #5138, #8243, #2584, #1302 ) ) ;
#1154 = ADVANCED_FACE ( 'NONE', ( #795 ), #2947, .T. ) ;
#1155 = ORIENTED_EDGE ( 'NONE', *, *, #12673, .T. ) ;
#1156 = EDGE_CURVE ( 'NONE', #12208, #9851, #8613, .T. ) ;
#1157 = CIRCLE ( 'NONE', #6908, 2.000000000000001776 ) ;
#1158 = DIRECTION ( 'NONE',  ( 0.000000000000000000, 1.000000000000000000, 0.000000000000000000 ) ) ;
#1159 = DIRECTION ( 'NONE',  ( -0.000000000000000000, -1.000000000000000000, 0.000000000000000000 ) ) ;
#1160 = CARTESIAN_POINT ( 'NONE',  ( 196.2980642835735239, 20.08915143291160632, -172.1812796681614941 ) ) ;
#1161 = CARTESIAN_POINT ( 'NONE',  ( 3.196328145774592416E-14, 20.00000000000000000, 261.0000000000000000 ) ) ;
#1162 = DIRECTION ( 'NONE',  ( 1.000000000000000000, 0.000000000000000000, 0.000000000000000000 ) ) ;
#1163 = CARTESIAN_POINT ( 'NONE',  ( -241.0949697661349376, 4.988078589341720992, 10.64105268566328100 ) ) ;
#1164 =( REPRESENTATION_RELATIONSHIP ('NONE','NONE', #12019, #182 ) REPRESENTATION_RELATIONSHIP_WITH_TRANSFORMATION ( #3071 )SHAPE_REPRESENTATION_RELATIONSHIP( ) );
#1165 = EDGE_CURVE ( 'NONE', #5784, #12886, #861, .T. ) ;
#1166 = AXIS2_PLACEMENT_3D ( 'NONE', #11964, #2622, #4559 ) ;
#1167 = CIRCLE ( 'NONE', #2642, 249.2999999999999829 ) ;
#1168 = ORIENTED_EDGE ( 'NONE', *, *, #10750, .F. ) ;
#1169 = CARTESIAN_POINT ( 'NONE',  ( 83.86521783953214992, 20.79694577634647601, 247.0684411393755511 ) ) ;
#1170 = VERTEX_POINT ( 'NONE', #8929 ) ;
#1171 = CARTESIAN_POINT ( 'NONE',  ( 0.000000000000000000, 24.99999999999995737, -246.0000000000000000 ) ) ;
#1172 = VERTEX_POINT ( 'NONE', #10057 ) ;
#1173 = ORIENTED_EDGE ( 'NONE', *, *, #3195, .F. ) ;
#1174 = CONICAL_SURFACE ( 'NONE', #11826, 196.0000000000000000, 0.7853981633974758125 ) ;
#1175 = DIRECTION ( 'NONE',  ( 0.6368676505102707219, 0.000000000000000000, 0.7709731485165535192 ) ) ;
#1176 =( NAMED_UNIT ( * ) PLANE_ANGLE_UNIT ( ) SI_UNIT ( $, .RADIAN. ) );
#1177 = PRODUCT_DEFINITION_SHAPE ( 'NONE', 'NONE',  #13053 ) ;
#1178 = CARTESIAN_POINT ( 'NONE',  ( 239.4581646394653944, 1.471889791882278198, 3.175461175233341926 ) ) ;
#1179 = DIRECTION ( 'NONE',  ( 0.000000000000000000, 1.000000000000000000, 0.000000000000000000 ) ) ;
#1180 = CARTESIAN_POINT ( 'NONE',  ( -67.47543992451981865, 20.08915143297737060, -251.8100110699624281 ) ) ;
#1181 = CARTESIAN_POINT ( 'NONE',  ( 0.000000000000000000, 3.061616997868383141E-16, 0.000000000000000000 ) ) ;
#1182 = EDGE_CURVE ( 'NONE', #4229, #4886, #693, .T. ) ;
#1183 = EDGE_CURVE ( 'NONE', #8254, #10706, #5194, .T. ) ;
#1184 = ITEM_DEFINED_TRANSFORMATION ( 'NONE', 'NONE', #11463,  #805 ) ;
#1185 = VERTEX_POINT ( 'NONE', #8396 ) ;
#1186 = DIRECTION ( 'NONE',  ( 1.000000000000000000, 0.000000000000000000, 0.000000000000000000 ) ) ;
#1187 = CIRCLE ( 'NONE', #8225, 6.500000000000005329 ) ;
#1188 = ORIENTED_EDGE ( 'NONE', *, *, #8602, .F. ) ;
#1189 = VECTOR ( 'NONE', #11301, 1000.000000000000000 ) ;
#1190 = CARTESIAN_POINT ( 'NONE',  ( 0.000000000000000000, 20.00000000000000000, -261.0000000000000000 ) ) ;
#1191 = DIRECTION ( 'NONE',  ( 0.000000000000000000, 1.000000000000000000, 0.000000000000000000 ) ) ;
#1192 = CARTESIAN_POINT ( 'NONE',  ( -249.6835501129397983, -11.19967427123757453, 3.553901704592668853 ) ) ;
#1193 = ORIENTED_EDGE ( 'NONE', *, *, #6647, .T. ) ;
#1194 = CARTESIAN_POINT ( 'NONE',  ( -207.3438552936920019, 20.79694577614539597, 159.0697709845790087 ) ) ;
#1195 = CARTESIAN_POINT ( 'NONE',  ( -244.6143483605412712, 8.518413540729250499, -8.452629823371180962 ) ) ;
#1196 = DIRECTION ( 'NONE',  ( 0.6368676505102707219, 0.000000000000000000, 0.7709731485165535192 ) ) ;
#1197 = CARTESIAN_POINT ( 'NONE',  ( -246.2885828969133684, -9.329251179348061029, -7.144935779693829758 ) ) ;
#1198 = AXIS2_PLACEMENT_3D ( 'NONE', #7541, #6348, #213 ) ;
#1199 = ADVANCED_FACE ( 'NONE', ( #6721 ), #10305, .F. ) ;
#1200 = DIRECTION ( 'NONE',  ( 0.000000000000000000, 1.000000000000000000, 0.000000000000000000 ) ) ;
#1201 = DIRECTION ( 'NONE',  ( 0.1736481776669404620, 0.000000000000000000, -0.9848077530122062440 ) ) ;
#1202 = CARTESIAN_POINT ( 'NONE',  ( 240.6009466513641541, 3.417710891856967859, -0.7616916529149476700 ) ) ;
#1203 = CARTESIAN_POINT ( 'NONE',  ( -289.8128292627096130, -19.40000000000000213, 10.41748504886635907 ) ) ;
#1204 = ORIENTED_EDGE ( 'NONE', *, *, #8795, .F. ) ;
#1205 = CARTESIAN_POINT ( 'NONE',  ( 17.05314194195614874, 20.08915143307225648, 260.5542428346390125 ) ) ;
#1206 = DIRECTION ( 'NONE',  ( 0.000000000000000000, 1.000000000000000000, 0.000000000000000000 ) ) ;
#1207 = CARTESIAN_POINT ( 'NONE',  ( -249.6746543471935809, 11.17527903294265279, 3.629830555898323929 ) ) ;
#1208 = FACE_OUTER_BOUND ( 'NONE', #353, .T. ) ;
#1209 = CARTESIAN_POINT ( 'NONE',  ( 0.000000000000000000, 0.000000000000000000, 0.000000000000000000 ) ) ;
#1210 = DIRECTION ( 'NONE',  ( 0.000000000000000000, -1.000000000000000000, 0.000000000000000000 ) ) ;
#1211 = DIRECTION ( 'NONE',  ( 0.000000000000000000, 0.8757116489157734662, 0.4828344519120573719 ) ) ;
#1212 = CARTESIAN_POINT ( 'NONE',  ( 0.000000000000000000, 0.000000000000000000, 0.000000000000000000 ) ) ;
#1213 = FACE_OUTER_BOUND ( 'NONE', #9627, .T. ) ;
#1214 = CONTEXT_DEPENDENT_SHAPE_REPRESENTATION ( #1845, #5054 ) ;
#1215 = ORIENTED_EDGE ( 'NONE', *, *, #6502, .F. ) ;
#1216 = DIRECTION ( 'NONE',  ( 0.000000000000000000, 1.000000000000000000, 0.000000000000000000 ) ) ;
#1217 = CARTESIAN_POINT ( 'NONE',  ( 229.9799928493307846, -1.755858631984955398, -3.036273278599403103 ) ) ;
#1218 = VERTEX_POINT ( 'NONE', #9698 ) ;
#1219 = ORIENTED_EDGE ( 'NONE', *, *, #10968, .T. ) ;
#1220 = CARTESIAN_POINT ( 'NONE',  ( 240.2701176883056178, -2.464548987107058942, 2.493043655918042667 ) ) ;
#1221 = DIRECTION ( 'NONE',  ( 0.6368676505102708330, 0.000000000000000000, 0.7709731485165535192 ) ) ;
#1222 = CARTESIAN_POINT ( 'NONE',  ( 17.09264059776268851, 19.96883746064459331, 261.1558126970361400 ) ) ;
#1223 = TOROIDAL_SURFACE ( 'NONE', #12290, 2.200000000000000178, 0.8000000000000000444 ) ;
#1224 = CARTESIAN_POINT ( 'NONE',  ( -229.2637990951503753, -30.00000000000000000, 180.9540284836414514 ) ) ;
#1225 = CARTESIAN_POINT ( 'NONE',  ( 0.000000000000000000, 0.000000000000000000, 0.000000000000000000 ) ) ;
#1226 = CARTESIAN_POINT ( 'NONE',  ( -240.1208361041844910, 2.772967769358974710, 11.41810622433049893 ) ) ;
#1227 = EDGE_CURVE ( 'NONE', #6293, #12220, #7581, .T. ) ;
#1228 = ADVANCED_FACE ( 'NONE', ( #7706, #1712 ), #455, .F. ) ;
#1229 = EDGE_LOOP ( 'NONE', ( #13019, #234 ) ) ;
#1230 = CARTESIAN_POINT ( 'NONE',  ( 212.0849693193239602, 20.79694577634646890, 151.9741924115231484 ) ) ;
#1231 = ORIENTED_EDGE ( 'NONE', *, *, #3028, .T. ) ;
#1232 = CARTESIAN_POINT ( 'NONE',  ( 0.000000000000000000, -2.772967769359314882, -240.3921568627448551 ) ) ;
#1233 = ORIENTED_EDGE ( 'NONE', *, *, #8587, .T. ) ;
#1234 = ORIENTED_EDGE ( 'NONE', *, *, #895, .T. ) ;
#1235 =( GEOMETRIC_REPRESENTATION_CONTEXT ( 3 ) GLOBAL_UNCERTAINTY_ASSIGNED_CONTEXT ( ( #7985 ) ) GLOBAL_UNIT_ASSIGNED_CONTEXT ( ( #9750, #8765, #5565 ) ) REPRESENTATION_CONTEXT ( 'NONE', 'WORKASPACE' ) );
#1236 = CARTESIAN_POINT ( 'NONE',  ( -0.000000000000000000, -1.848645179577135034, 0.000000000000000000 ) ) ;
#1237 = LINE ( 'NONE', #8445, #7442 ) ;
#1238 = CARTESIAN_POINT ( 'NONE',  ( -225.1241593668336236, -18.00000000000000000, 185.9653539489990521 ) ) ;
#1239 = DIRECTION ( 'NONE',  ( -0.000000000000000000, -1.000000000000000000, 0.000000000000000000 ) ) ;
#1240 = CARTESIAN_POINT ( 'NONE',  ( 0.000000000000000000, 0.000000000000000000, 0.000000000000000000 ) ) ;
#1241 = DIRECTION ( 'NONE',  ( 0.000000000000000000, 0.000000000000000000, 1.000000000000000000 ) ) ;
#1242 = AXIS2_PLACEMENT_3D ( 'NONE', #1146, #6149, #5272 ) ;
#1243 = ITEM_DEFINED_TRANSFORMATION ( 'NONE', 'NONE', #2521,  #805 ) ;
#1244 = VERTEX_POINT ( 'NONE', #718 ) ;
#1245 = CARTESIAN_POINT ( 'NONE',  ( 71.82423009839129691, 28.60000000000000142, -197.3354503650404865 ) ) ;
#1246 = VERTEX_POINT ( 'NONE', #11720 ) ;
#1247 = DIRECTION ( 'NONE',  ( -0.000000000000000000, -1.000000000000000000, 0.000000000000000000 ) ) ;
#1248 = CARTESIAN_POINT ( 'NONE',  ( -246.2769436246209125, -9.326692435563586514, -7.550684327968305354 ) ) ;
#1249 = CARTESIAN_POINT ( 'NONE',  ( 34.02434144668549720, 20.08915143297735995, 258.4638482596384392 ) ) ;
#1250 = ORIENTED_EDGE ( 'NONE', *, *, #5677, .T. ) ;
#1251 = AXIS2_PLACEMENT_3D ( 'NONE', #9452, #3363, #11450 ) ;
#1252 = EDGE_CURVE ( 'NONE', #10483, #10082, #3490, .T. ) ;
#1253 = VECTOR ( 'NONE', #12788, 1000.000000000000000 ) ;
#1254 = CARTESIAN_POINT ( 'NONE',  ( 259.0935598587374784, 20.79694577687060786, 34.13493237085509691 ) ) ;
#1255 = ADVANCED_FACE ( 'NONE', ( #10775 ), #11745, .F. ) ;
#1256 = CARTESIAN_POINT ( 'NONE',  ( -240.5058532487275329, 3.857938722303589696, -11.36295048183480283 ) ) ;
#1257 = CARTESIAN_POINT ( 'NONE',  ( -238.8437317866286378, 0.8419213848770401576, 11.97081056113904651 ) ) ;
#1258 = AXIS2_PLACEMENT_3D ( 'NONE', #12752, #3616, #7684 ) ;
#1259 = CARTESIAN_POINT ( 'NONE',  ( -244.2871807278710889, -8.304201005131382374, -8.312831358495099465 ) ) ;
#1260 = CIRCLE ( 'NONE', #11042, 249.0000000000000284 ) ;
#1261 = VECTOR ( 'NONE', #7857, 1000.000000000000000 ) ;
#1262 = PRODUCT_CONTEXT ( 'NONE', #10454, 'mechanical' ) ;
#1263 = CARTESIAN_POINT ( 'NONE',  ( -229.7434709365983565, 5.107855674974426385, -10.86021397319516169 ) ) ;
#1264 = CONTEXT_DEPENDENT_SHAPE_REPRESENTATION ( #8097, #11648 ) ;
#1265 = AXIS2_PLACEMENT_3D ( 'NONE', #8906, #12976, #4769 ) ;
#1266 = VECTOR ( 'NONE', #8246, 1000.000000000000000 ) ;
#1267 = DIRECTION ( 'NONE',  ( 0.000000000000000000, -1.000000000000000000, 0.000000000000000000 ) ) ;
#1268 = ORIENTED_EDGE ( 'NONE', *, *, #8533, .T. ) ;
#1269 = CARTESIAN_POINT ( 'NONE',  ( -226.1171533162824971, 20.08915143300168893, 130.5770120869439950 ) ) ;
#1270 = EDGE_CURVE ( 'NONE', #7994, #1045, #2778, .T. ) ;
#1271 = DIRECTION ( 'NONE',  ( 0.000000000000000000, 0.000000000000000000, -1.000000000000000000 ) ) ;
#1272 = DIRECTION ( 'NONE',  ( -0.4503334343941627904, -0.7071067811865381358, -0.5451603414288054283 ) ) ;
#1273 = VECTOR ( 'NONE', #5631, 1000.000000000000000 ) ;
#1274 = CARTESIAN_POINT ( 'NONE',  ( -289.8128292627096130, -30.00000000000000000, 10.41748504886635907 ) ) ;
#1275 = CARTESIAN_POINT ( 'NONE',  ( -246.6520855341642289, -9.461709548621238142, 7.381047753367473874 ) ) ;
#1276 = AXIS2_PLACEMENT_3D ( 'NONE', #2445, #9456, #4381 ) ;
#1277 = ADVANCED_FACE ( 'NONE', ( #8845 ), #9181, .F. ) ;
#1278 = DIRECTION ( 'NONE',  ( 0.000000000000000000, 0.000000000000000000, 1.000000000000000000 ) ) ;
#1279 = DIRECTION ( 'NONE',  ( -3.491481338843133355E-15, 0.000000000000000000, 1.000000000000000000 ) ) ;
#1280 = CARTESIAN_POINT ( 'NONE',  ( 228.6269314446401211, -19.00000000000000000, -181.7250016321579835 ) ) ;
#1281 = VERTEX_POINT ( 'NONE', #6524 ) ;
#1282 =( REPRESENTATION_RELATIONSHIP ('NONE','NONE', #12019, #5191 ) REPRESENTATION_RELATIONSHIP_WITH_TRANSFORMATION ( #11602 )SHAPE_REPRESENTATION_RELATIONSHIP( ) );
#1283 = CARTESIAN_POINT ( 'NONE',  ( 71.82423009839129691, 18.00000000000000000, -197.3354503650404865 ) ) ;
#1284 = VECTOR ( 'NONE', #12599, 1000.000000000000000 ) ;
#1285 = PRODUCT_DEFINITION_SHAPE ( 'NONE', 'NONE',  #13074 ) ;
#1286 = CARTESIAN_POINT ( 'NONE',  ( 230.0000012283371973, -3.500080719304503596, -0.2270454585753299837 ) ) ;
#1287 = ORIENTED_EDGE ( 'NONE', *, *, #512, .T. ) ;
#1288 = EDGE_LOOP ( 'NONE', ( #7427, #8375, #2289, #5621 ) ) ;
#1289 = FACE_OUTER_BOUND ( 'NONE', #12054, .T. ) ;
#1290 = FACE_OUTER_BOUND ( 'NONE', #10006, .T. ) ;
#1291 = AXIS2_PLACEMENT_3D ( 'NONE', #4047, #3040, #8259 ) ;
#1292 = CARTESIAN_POINT ( 'NONE',  ( -130.9697226067400493, 20.55460285172577883, 226.7975291057999527 ) ) ;
#1293 = DIRECTION ( 'NONE',  ( -0.6368676505102707219, 0.000000000000000000, -0.7709731485165536302 ) ) ;
#1294 = DIRECTION ( 'NONE',  ( -0.7660444431189792347, 0.000000000000000000, 0.6427876096865379196 ) ) ;
#1295 = LINE ( 'NONE', #4355, #1995 ) ;
#1296 = AXIS2_PLACEMENT_3D ( 'NONE', #1328, #8336, #4385 ) ;
#1297 = ORIENTED_EDGE ( 'NONE', *, *, #6841, .F. ) ;
#1298 = CARTESIAN_POINT ( 'NONE',  ( 0.000000000000000000, 11.79660968244690089, 247.7999999999999829 ) ) ;
#1299 = ORIENTED_EDGE ( 'NONE', *, *, #201, .F. ) ;
#1300 = FACE_OUTER_BOUND ( 'NONE', #2873, .T. ) ;
#1301 = EDGE_LOOP ( 'NONE', ( #12296, #7141, #10815, #12253 ) ) ;
#1302 = ORIENTED_EDGE ( 'NONE', *, *, #2252, .F. ) ;
#1303 = EDGE_CURVE ( 'NONE', #5861, #10423, #3419, .T. ) ;
#1304 = DIRECTION ( 'NONE',  ( -0.000000000000000000, -1.000000000000000000, 0.000000000000000000 ) ) ;
#1305 = VECTOR ( 'NONE', #8021, 1000.000000000000000 ) ;
#1306 = CARTESIAN_POINT ( 'NONE',  ( 226.7234983661818717, 0.000000000000000000, 0.000000000000000000 ) ) ;
#1307 = CARTESIAN_POINT ( 'NONE',  ( -225.1241593668336236, -30.00000000000000000, 185.9653539489990521 ) ) ;
#1308 = CARTESIAN_POINT ( 'NONE',  ( -239.2756820386164804, 1.575831832474349437, -11.64383448413514976 ) ) ;
#1309 = CARTESIAN_POINT ( 'NONE',  ( -247.0236966368111950, 9.579141830482246434, 7.227478268527401717 ) ) ;
#1310 = DIRECTION ( 'NONE',  ( -0.5024607274629890874, -0.3950277506594149224, 0.7690814609430699500 ) ) ;
#1311 = AXIS2_PLACEMENT_3D ( 'NONE', #11230, #5029, #2097 ) ;
#1312 = ORIENTED_EDGE ( 'NONE', *, *, #4894, .T. ) ;
#1313 = FACE_OUTER_BOUND ( 'NONE', #12183, .T. ) ;
#1314 = CARTESIAN_POINT ( 'NONE',  ( 153.9282213272189495, -28.60000000000000142, 245.7765299597151341 ) ) ;
#1315 = ORIENTED_EDGE ( 'NONE', *, *, #3096, .T. ) ;
#1316 = PRODUCT_DEFINITION_SHAPE ( 'NONE', 'NONE',  #13187 ) ;
#1317 = CARTESIAN_POINT ( 'NONE',  ( 227.3999999999999773, -2.326370887777457153, -3.852012265362291465 ) ) ;
#1318 = LINE ( 'NONE', #4501, #9779 ) ;
#1319 = CARTESIAN_POINT ( 'NONE',  ( 221.3800702329289720, 20.08915143297736705, 137.6665579279351732 ) ) ;
#1320 = ORIENTED_EDGE ( 'NONE', *, *, #10196, .T. ) ;
#1321 = EDGE_CURVE ( 'NONE', #1858, #4661, #11845, .T. ) ;
#1322 = CARTESIAN_POINT ( 'NONE',  ( 235.4000000000000057, 0.000000000000000000, 0.000000000000000000 ) ) ;
#1323 = CARTESIAN_POINT ( 'NONE',  ( -245.3145835528066812, 8.904103459659600261, -8.045132556734525764 ) ) ;
#1324 = CARTESIAN_POINT ( 'NONE',  ( -238.6985546676629326, 0.1065515246389758391, 11.99999998203097107 ) ) ;
#1325 = CARTESIAN_POINT ( 'NONE',  ( 158.0678610555357295, -30.00000000000000000, 250.7878554250727632 ) ) ;
#1326 = CIRCLE ( 'NONE', #9834, 5.500000000000005329 ) ;
#1327 = CARTESIAN_POINT ( 'NONE',  ( 0.000000000000000000, 20.00000000000000000, 0.000000000000000000 ) ) ;
#1328 = CARTESIAN_POINT ( 'NONE',  ( 10.83189848055792659, -138.4705547276867321, 40.42519547187246332 ) ) ;
#1329 = EDGE_CURVE ( 'NONE', #2886, #5106, #6001, .T. ) ;
#1330 = CARTESIAN_POINT ( 'NONE',  ( -229.8368610672713146, 8.310328450785883447, -8.664835459456435629 ) ) ;
#1331 = CONTEXT_DEPENDENT_SHAPE_REPRESENTATION ( #11326, #3653 ) ;
#1332 = DIRECTION ( 'NONE',  ( 0.000000000000000000, 1.000000000000000000, 0.000000000000000000 ) ) ;
#1333 = EDGE_LOOP ( 'NONE', ( #4898, #4678 ) ) ;
#1334 = CARTESIAN_POINT ( 'NONE',  ( -247.8175805188620018, 19.96883746128897386, -84.14846197934974725 ) ) ;
#1335 = DIRECTION ( 'NONE',  ( 0.000000000000000000, 0.000000000000000000, 1.000000000000000000 ) ) ;
#1336 = CARTESIAN_POINT ( 'NONE',  ( 71.82423009839129691, 30.00000000000000000, -202.4354503650404808 ) ) ;
#1337 = CIRCLE ( 'NONE', #4945, 4.000000000000000000 ) ;
#1338 = CARTESIAN_POINT ( 'NONE',  ( 227.3999999999999773, -4.447920636657316074, 2.686261716586446635 ) ) ;
#1339 = DIRECTION ( 'NONE',  ( 0.000000000000000000, 0.000000000000000000, -1.000000000000000000 ) ) ;
#1340 = DIRECTION ( 'NONE',  ( 0.000000000000000000, -1.000000000000000000, 0.000000000000000000 ) ) ;
#1341 = CARTESIAN_POINT ( 'NONE',  ( -40.42519547187227857, -138.4705547276867321, -10.83189848055863180 ) ) ;
#1343 = ADVANCED_FACE ( 'NONE', ( #3765 ), #8341, .F. ) ;
#1342 = CIRCLE ( 'NONE', #9629, 10.00000000000000178 ) ;
#1344 = LINE ( 'NONE', #2470, #2225 ) ;
#1345 = CONTEXT_DEPENDENT_SHAPE_REPRESENTATION ( #2753, #12203 ) ;
#1346 = ADVANCED_FACE ( 'NONE', ( #6589 ), #8973, .F. ) ;
#1347 = EDGE_LOOP ( 'NONE', ( #9668, #11883, #1234, #3830 ) ) ;
#1348 = CIRCLE ( 'NONE', #1127, 10.00000000000000178 ) ;
#1349 = CARTESIAN_POINT ( 'NONE',  ( 240.5727840947570826, -3.342302961263916572, 1.043131940311951888 ) ) ;
#1350 = CARTESIAN_POINT ( 'NONE',  ( -229.9335310080516592, -10.65269000883797190, 5.546765194287003986 ) ) ;
#1351 = ORIENTED_EDGE ( 'NONE', *, *, #7739, .F. ) ;
#1352 = ORIENTED_EDGE ( 'NONE', *, *, #7689, .T. ) ;
#1353 = EDGE_CURVE ( 'NONE', #3016, #3738, #10239, .T. ) ;
#1354 = CARTESIAN_POINT ( 'NONE',  ( 240.1689872792144627, -2.295088600365091214, 2.642490611637378972 ) ) ;
#1355 = CARTESIAN_POINT ( 'NONE',  ( 197.8197553893915028, 30.00000000000000000, -64.27553482998990830 ) ) ;
#1356 = CONICAL_SURFACE ( 'NONE', #4960, 6.499999999999999112, 0.7853981633974476129 ) ;
#1357 = AXIS2_PLACEMENT_3D ( 'NONE', #1245, #5311, #10510 ) ;
#1358 = CARTESIAN_POINT ( 'NONE',  ( -247.9906035367588402, 20.55460285060343040, -84.20717312374212327 ) ) ;
#1359 = CARTESIAN_POINT ( 'NONE',  ( 153.9282213272189495, -30.00000000000000000, 245.7765299597151341 ) ) ;
#1360 = CARTESIAN_POINT ( 'NONE',  ( 0.000000000000000000, 0.000000000000000000, 0.000000000000000000 ) ) ;
#1361 = CARTESIAN_POINT ( 'NONE',  ( 2.388061258337338860E-14, 0.000000000000000000, 195.0000000000000000 ) ) ;
#1362 = CARTESIAN_POINT ( 'NONE',  ( -221.5672498511021900, 20.79694577634646180, 137.7829567244527880 ) ) ;
#1363 = EDGE_CURVE ( 'NONE', #4210, #8633, #7270, .T. ) ;
#1364 = ORIENTED_EDGE ( 'NONE', *, *, #10626, .T. ) ;
#1365 = CARTESIAN_POINT ( 'NONE',  ( 158.8368823490025932, 20.79694577634646890, -206.9952515782967737 ) ) ;
#1366 = CIRCLE ( 'NONE', #2001, 2.000000000000001776 ) ;
#1367 = ORIENTED_EDGE ( 'NONE', *, *, #1628, .F. ) ;
#1368 = CARTESIAN_POINT ( 'NONE',  ( -248.0831933713610056, -9.830508068705260172, -6.436117704883899115 ) ) ;
#1369 = ORIENTED_EDGE ( 'NONE', *, *, #2578, .T. ) ;
#1370 = VERTEX_POINT ( 'NONE', #8711 ) ;
#1371 = VECTOR ( 'NONE', #3321, 1000.000000000000114 ) ;
#1372 = CARTESIAN_POINT ( 'NONE',  ( 158.0678610555357295, -30.00000000000000000, 250.7878554250727632 ) ) ;
#1373 = CARTESIAN_POINT ( 'NONE',  ( 235.4000000000000057, 0.000000000000000000, 0.000000000000000000 ) ) ;
#1374 = CARTESIAN_POINT ( 'NONE',  ( 0.000000000000000000, 19.00000000000000000, -208.0000000000000000 ) ) ;
#1375 = CONICAL_SURFACE ( 'NONE', #4547, 249.7999999999999829, 0.7853981633975309906 ) ;
#1376 = CARTESIAN_POINT ( 'NONE',  ( -239.2239425775430561, 1.510213393934768833, -11.65254303168215522 ) ) ;
#1377 = TOROIDAL_SURFACE ( 'NONE', #12236, 261.5294117647060261, 2.000000000000000000 ) ;
#1378 = DIRECTION ( 'NONE',  ( -0.6368676505102698338, 0.000000000000000000, -0.7709731485165542964 ) ) ;
#1379 = CONTEXT_DEPENDENT_SHAPE_REPRESENTATION ( #2075, #3063 ) ;
#1380 = EDGE_LOOP ( 'NONE', ( #12699, #5639, #6225, #9706 ) ) ;
#1381 = CARTESIAN_POINT ( 'NONE',  ( 185.9653539490014111, -30.00000000000000000, 225.1241593668316625 ) ) ;
#1382 = ORIENTED_EDGE ( 'NONE', *, *, #10215, .T. ) ;
#1383 = CARTESIAN_POINT ( 'NONE',  ( 0.000000000000000000, 0.000000000000000000, -195.0000000000000000 ) ) ;
#1384 = CARTESIAN_POINT ( 'NONE',  ( 0.000000000000000000, 19.00000000000000000, 0.000000000000000000 ) ) ;
#1385 = AXIS2_PLACEMENT_3D ( 'NONE', #2580, #5716, #2641 ) ;
#1386 = CARTESIAN_POINT ( 'NONE',  ( 206.8203823583190228, 20.08915143297735995, -158.7026972336033737 ) ) ;
#1387 = DIRECTION ( 'NONE',  ( 1.000000000000000000, 0.000000000000000000, 0.000000000000000000 ) ) ;
#1388 = CARTESIAN_POINT ( 'NONE',  ( -244.8752249706953990, 8.669362157675379876, -8.297136228722845175 ) ) ;
#1389 = CARTESIAN_POINT ( 'NONE',  ( 0.000000000000000000, 18.00000000000000000, 208.0000000000000000 ) ) ;
#1390 = CARTESIAN_POINT ( 'NONE',  ( -239.5361044668159991, -1.848645179572815156, -11.60366368868215758 ) ) ;
#1391 = AXIS2_PLACEMENT_3D ( 'NONE', #6939, #11192, #2057 ) ;
#1392 = LINE ( 'NONE', #8528, #8634 ) ;
#1393 = PRODUCT ( 'Ball Separator Polymer', 'Ball Separator Polymer', '', ( #5394 ) ) ;
#1394 = DIRECTION ( 'NONE',  ( 1.000000000000000000, 0.000000000000000000, 0.000000000000000000 ) ) ;
#1395 = CIRCLE ( 'NONE', #9275, 245.7999999999999829 ) ;
#1396 = EDGE_CURVE ( 'NONE', #9887, #982, #5515, .T. ) ;
#1397 = CARTESIAN_POINT ( 'NONE',  ( -229.8757030161491741, 9.332370542760813237, -7.580342957207111709 ) ) ;
#1398 = ADVANCED_FACE ( 'NONE', ( #1640 ), #3211, .F. ) ;
#1399 = CONTEXT_DEPENDENT_SHAPE_REPRESENTATION ( #3566, #6430 ) ;
#1400 = CARTESIAN_POINT ( 'NONE',  ( 235.4000000000000057, 3.999223041228192610, -0.07883569311883599495 ) ) ;
#1401 = VERTEX_POINT ( 'NONE', #9042 ) ;
#1402 = VECTOR ( 'NONE', #5824, 1000.000000000000114 ) ;
#1403 = CARTESIAN_POINT ( 'NONE',  ( 115.7315435905548071, 19.96883745941821786, 234.7354397751816180 ) ) ;
#1404 = DIRECTION ( 'NONE',  ( 0.000000000000000000, -1.000000000000000000, 0.000000000000000000 ) ) ;
#1405 = CYLINDRICAL_SURFACE ( 'NONE', #6256, 5.500000000000007994 ) ;
#1406 =( REPRESENTATION_RELATIONSHIP ('NONE','NONE', #12019, #182 ) REPRESENTATION_RELATIONSHIP_WITH_TRANSFORMATION ( #1113 )SHAPE_REPRESENTATION_RELATIONSHIP( ) );
#1407 = FACE_OUTER_BOUND ( 'NONE', #12837, .T. ) ;
#1408 = CARTESIAN_POINT ( 'NONE',  ( -233.8077470125392949, 20.08915143297735995, 115.3046144132251101 ) ) ;
#1409 = DIRECTION ( 'NONE',  ( -0.000000000000000000, -1.000000000000000000, 0.000000000000000000 ) ) ;
#1410 = CARTESIAN_POINT ( 'NONE',  ( -36.24423871767969274, -138.4705547276867321, -20.92562098022565209 ) ) ;
#1411 = CARTESIAN_POINT ( 'NONE',  ( -246.1720478449190637, -9.282004955874285201, 7.205195110361622746 ) ) ;
#1412 = ITEM_DEFINED_TRANSFORMATION ( 'NONE', 'NONE', #2349,  #805 ) ;
#1413 = DIRECTION ( 'NONE',  ( -0.000000000000000000, -1.000000000000000000, 0.000000000000000000 ) ) ;
#1414 = DIRECTION ( 'NONE',  ( 8.659560562354926695E-17, 0.7071067811865480168, -0.7071067811865470176 ) ) ;
#1415 = ORIENTED_EDGE ( 'NONE', *, *, #3005, .F. ) ;
#1416 = VERTEX_POINT ( 'NONE', #11976 ) ;
#1417 = LINE ( 'NONE', #12611, #8489 ) ;
#1418 = CARTESIAN_POINT ( 'NONE',  ( 0.000000000000000000, -25.00000000000000000, 0.000000000000000000 ) ) ;
#1419 = EDGE_CURVE ( 'NONE', #10498, #2672, #1090, .T. ) ;
#1420 = EDGE_CURVE ( 'NONE', #2835, #10938, #4844, .T. ) ;
#1421 = CARTESIAN_POINT ( 'NONE',  ( -1.008906662707803564E-12, 19.96883746059272724, 261.1558126970361400 ) ) ;
#1422 = DIRECTION ( 'NONE',  ( 0.000000000000000000, 0.000000000000000000, -1.000000000000000000 ) ) ;
#1423 = CARTESIAN_POINT ( 'NONE',  ( 0.000000000000000000, 0.000000000000000000, 0.000000000000000000 ) ) ;
#1424 = CARTESIAN_POINT ( 'NONE',  ( -240.8352866734745419, 4.521734055696428278, 10.84609021980019250 ) ) ;
#1425 = CARTESIAN_POINT ( 'NONE',  ( -151.9741924115236031, 20.79694577634646180, 212.0849693193235055 ) ) ;
#1426 = ORIENTED_EDGE ( 'NONE', *, *, #3118, .T. ) ;
#1427 = CARTESIAN_POINT ( 'NONE',  ( 252.0229195836993199, 20.79694577634646535, -67.53249125288874666 ) ) ;
#1428 = ORIENTED_EDGE ( 'NONE', *, *, #4125, .T. ) ;
#1429 = AXIS2_PLACEMENT_3D ( 'NONE', #12612, #4348, #11623 ) ;
#1430 = FACE_OUTER_BOUND ( 'NONE', #10359, .T. ) ;
#1431 = VERTEX_POINT ( 'NONE', #13015 ) ;
#1432 = VERTEX_POINT ( 'NONE', #6975 ) ;
#1433 = DIRECTION ( 'NONE',  ( -0.000000000000000000, -1.000000000000000000, 0.000000000000000000 ) ) ;
#1434 = EDGE_CURVE ( 'NONE', #5762, #8072, #10667, .T. ) ;
#1435 = CARTESIAN_POINT ( 'NONE',  ( -210.0000000000000000, 30.00000000000000000, 6.500000000000000000 ) ) ;
#1436 = DIRECTION ( 'NONE',  ( 1.000000000000000000, 0.000000000000000000, 0.000000000000000000 ) ) ;
#1437 = CYLINDRICAL_SURFACE ( 'NONE', #7753, 270.0000000000000000 ) ;
#1438 = DIRECTION ( 'NONE',  ( 0.000000000000000000, -1.000000000000000000, 0.000000000000000000 ) ) ;
#1439 = EDGE_CURVE ( 'NONE', #953, #4809, #1519, .T. ) ;
#1440 = ITEM_DEFINED_TRANSFORMATION ( 'NONE', 'NONE', #7626,  #805 ) ;
#1441 = ORIENTED_EDGE ( 'NONE', *, *, #2466, .F. ) ;
#1442 = CARTESIAN_POINT ( 'NONE',  ( 71.82423009839129691, 19.40000000000000213, -197.3354503650404865 ) ) ;
#1444 = ORIENTED_EDGE ( 'NONE', *, *, #4920, .T. ) ;
#1443 = VECTOR ( 'NONE', #8797, 1000.000000000000000 ) ;
#1445 = CARTESIAN_POINT ( 'NONE',  ( 0.000000000000000000, 0.000000000000000000, -230.0000000000000000 ) ) ;
#1446 = FACE_OUTER_BOUND ( 'NONE', #2903, .T. ) ;
#1447 = DIRECTION ( 'NONE',  ( -0.000000000000000000, -1.000000000000000000, 0.000000000000000000 ) ) ;
#1448 = DIRECTION ( 'NONE',  ( 0.000000000000000000, 0.000000000000000000, 1.000000000000000000 ) ) ;
#1449 = DIRECTION ( 'NONE',  ( 0.000000000000000000, 0.000000000000000000, 1.000000000000000000 ) ) ;
#1450 = CARTESIAN_POINT ( 'NONE',  ( -229.7744328040709263, 5.870883422401756313, 10.18542137201373166 ) ) ;
#1451 =( GEOMETRIC_REPRESENTATION_CONTEXT ( 3 ) GLOBAL_UNCERTAINTY_ASSIGNED_CONTEXT ( ( #7357 ) ) GLOBAL_UNIT_ASSIGNED_CONTEXT ( ( #9033, #8833, #10287 ) ) REPRESENTATION_CONTEXT ( 'NONE', 'WORKASPACE' ) );
#1452 = DIRECTION ( 'NONE',  ( 0.6368676505102689456, 0.000000000000000000, 0.7709731485165549625 ) ) ;
#1453 = CARTESIAN_POINT ( 'NONE',  ( -229.8756056487268324, 9.317215184761726832, 7.564809101436958727 ) ) ;
#1454 = ITEM_DEFINED_TRANSFORMATION ( 'NONE', 'NONE', #11727,  #805 ) ;
#1455 = AXIS2_PLACEMENT_3D ( 'NONE', #2024, #7289, #3140 ) ;
#1456 = AXIS2_PLACEMENT_3D ( 'NONE', #5382, #2248, #10445 ) ;
#1457 = CONICAL_SURFACE ( 'NONE', #6578, 5.500000000000015099, 0.7853981633974461696 ) ;
#1458 = AXIS2_PLACEMENT_3D ( 'NONE', #11202, #7145, #2922 ) ;
#1459 = AXIS2_PLACEMENT_3D ( 'NONE', #300, #361, #11492 ) ;
#1460 = DIRECTION ( 'NONE',  ( 0.000000000000000000, -1.000000000000000000, 0.000000000000000000 ) ) ;
#1461 = AXIS2_PLACEMENT_3D ( 'NONE', #10142, #7221, #4277 ) ;
#1462 = VERTEX_POINT ( 'NONE', #3835 ) ;
#1463 = CARTESIAN_POINT ( 'NONE',  ( -159.3024069663917146, 19.96883746063718590, -207.6469600136618681 ) ) ;
#1464 = DIRECTION ( 'NONE',  ( 0.000000000000000000, 0.000000000000000000, 1.000000000000000000 ) ) ;
#1465 = CARTESIAN_POINT ( 'NONE',  ( 225.1241593668336236, -30.00000000000000000, -185.9653539489990521 ) ) ;
#1466 = EDGE_CURVE ( 'NONE', #4307, #889, #11101, .T. ) ;
#1467 = FACE_OUTER_BOUND ( 'NONE', #967, .T. ) ;
#1468 = CARTESIAN_POINT ( 'NONE',  ( 0.000000000000000000, 0.000000000000000000, 3.499999999999964917 ) ) ;
#1469 = VECTOR ( 'NONE', #10856, 1000.000000000000000 ) ;
#1470 = DIRECTION ( 'NONE',  ( 1.000000000000000000, 0.000000000000000000, 0.000000000000000000 ) ) ;
#1471 = DIRECTION ( 'NONE',  ( -0.7823834078220617272, 0.5538822189107472926, -0.2847642722309892682 ) ) ;
#1472 = CARTESIAN_POINT ( 'NONE',  ( -229.6996680450365034, 7.200459016985159977E-17, -11.75000000000000000 ) ) ;
#1473 = AXIS2_PLACEMENT_3D ( 'NONE', #5369, #5234, #10298 ) ;
#1474 = DIRECTION ( 'NONE',  ( -0.000000000000000000, -1.000000000000000000, 0.000000000000000000 ) ) ;
#1475 = CIRCLE ( 'NONE', #3813, 5.500000000000005329 ) ;
#1476 =( REPRESENTATION_RELATIONSHIP ('NONE','NONE', #12019, #5191 ) REPRESENTATION_RELATIONSHIP_WITH_TRANSFORMATION ( #12929 )SHAPE_REPRESENTATION_RELATIONSHIP( ) );
#1477 = CARTESIAN_POINT ( 'NONE',  ( 0.000000000000000000, 25.00000000000000000, 0.000000000000000000 ) ) ;
#1478 = ORIENTED_EDGE ( 'NONE', *, *, #3171, .F. ) ;
#1479 = ORIENTED_EDGE ( 'NONE', *, *, #5493, .F. ) ;
#1480 = CIRCLE ( 'NONE', #2326, 2.500000000000002220 ) ;
#1481 = DIRECTION ( 'NONE',  ( 0.000000000000000000, 1.000000000000000000, 0.000000000000000000 ) ) ;
#1482 = FACE_OUTER_BOUND ( 'NONE', #7898, .T. ) ;
#1483 = EDGE_CURVE ( 'NONE', #10156, #5993, #12381, .T. ) ;
#1484 = CARTESIAN_POINT ( 'NONE',  ( 261.1558126970361400, 19.96883746059272724, 17.09264059808175062 ) ) ;
#1485 = DIRECTION ( 'NONE',  ( 0.000000000000000000, 0.000000000000000000, -1.000000000000000000 ) ) ;
#1486 = DIRECTION ( 'NONE',  ( 0.5735764363510443831, 0.000000000000000000, 0.8191520442889930198 ) ) ;
#1487 = FACE_OUTER_BOUND ( 'NONE', #6503, .T. ) ;
#1488 = CARTESIAN_POINT ( 'NONE',  ( -206.9952515782971716, 20.79694577634646535, 158.8368823490019395 ) ) ;
#1489 = AXIS2_PLACEMENT_3D ( 'NONE', #4138, #8410, #12472 ) ;
#1490 = ORIENTED_EDGE ( 'NONE', *, *, #4901, .F. ) ;
#1491 = CARTESIAN_POINT ( 'NONE',  ( -245.7999999999999829, 25.00000000000000000, 0.000000000000000000 ) ) ;
#1492 = EDGE_CURVE ( 'NONE', #13031, #5207, #5774, .T. ) ;
#1493 = ORIENTED_EDGE ( 'NONE', *, *, #10882, .T. ) ;
#1494 = ADVANCED_FACE ( 'NONE', ( #2962 ), #8547, .F. ) ;
#1495 = CARTESIAN_POINT ( 'NONE',  ( -23.54981712579610331, -30.00000000000000000, 295.6955080056604288 ) ) ;
#1496 = EDGE_LOOP ( 'NONE', ( #3668, #5704 ) ) ;
#1497 = EDGE_LOOP ( 'NONE', ( #1168, #4643, #11486, #3417 ) ) ;
#1498 = DIRECTION ( 'NONE',  ( 0.000000000000000000, 0.000000000000000000, 1.000000000000000000 ) ) ;
#1499 = DIRECTION ( 'NONE',  ( -0.000000000000000000, -1.000000000000000000, 0.000000000000000000 ) ) ;
#1500 = CARTESIAN_POINT ( 'NONE',  ( 239.5749691958646963, 1.619550704603064384, -3.102778355204328875 ) ) ;
#1501 = AXIS2_PLACEMENT_3D ( 'NONE', #2985, #10255, #6201 ) ;
#1502 = CARTESIAN_POINT ( 'NONE',  ( -239.0190616670419672, 1.196899100009489958, -11.68891583568077763 ) ) ;
#1503 = DIRECTION ( 'NONE',  ( 0.000000000000000000, 1.000000000000000000, 0.000000000000000000 ) ) ;
#1504 = AXIS2_PLACEMENT_3D ( 'NONE', #5276, #10479, #6351 ) ;
#1505 = VERTEX_POINT ( 'NONE', #7043 ) ;
#1506 = DIRECTION ( 'NONE',  ( 0.6368676505102716101, 0.000000000000000000, 0.7709731485165527420 ) ) ;
#1507 = EDGE_CURVE ( 'NONE', #10768, #8072, #5850, .T. ) ;
#1508 =( REPRESENTATION_RELATIONSHIP ('NONE','NONE', #12019, #5191 ) REPRESENTATION_RELATIONSHIP_WITH_TRANSFORMATION ( #7666 )SHAPE_REPRESENTATION_RELATIONSHIP( ) );
#1509 = EDGE_LOOP ( 'NONE', ( #8706, #2553 ) ) ;
#1510 = EDGE_CURVE ( 'NONE', #10886, #4193, #11315, .T. ) ;
#1511 = CARTESIAN_POINT ( 'NONE',  ( -242.2606306443440758, 6.568547307491611420, -9.743049585709520954 ) ) ;
#1512 = DIRECTION ( 'NONE',  ( 0.000000000000000000, 1.000000000000000000, 0.000000000000000000 ) ) ;
#1513 = AXIS2_PLACEMENT_3D ( 'NONE', #11806, #4647, #6800 ) ;
#1514 = EDGE_CURVE ( 'NONE', #1648, #171, #11908, .T. ) ;
#1515 = FACE_OUTER_BOUND ( 'NONE', #11834, .T. ) ;
#1516 = DIRECTION ( 'NONE',  ( 0.000000000000000000, 1.000000000000000000, 0.000000000000000000 ) ) ;
#1517 = CARTESIAN_POINT ( 'NONE',  ( -240.6986105848272359, -4.249529545660171159, -10.95469206485073421 ) ) ;
#1518 = FACE_OUTER_BOUND ( 'NONE', #11567, .T. ) ;
#1519 = CIRCLE ( 'NONE', #3641, 251.5674242726969680 ) ;
#1520 = AXIS2_PLACEMENT_3D ( 'NONE', #2880, #9030, #4018 ) ;
#1521 = DIRECTION ( 'NONE',  ( 0.7709731485165535192, 0.000000000000000000, -0.6368676505102707219 ) ) ;
#1522 = APPLICATION_PROTOCOL_DEFINITION ( 'draft international standard', 'automotive_design', 1998, #5679 ) ;
#1523 = CARTESIAN_POINT ( 'NONE',  ( -229.9999846513224782, 11.99971501660928297, 0.7499535807134399823 ) ) ;
#1524 = EDGE_CURVE ( 'NONE', #8945, #4077, #11104, .T. ) ;
#1525 = MANIFOLD_SOLID_BREP ( 'NONE', #716 ) ;
#1526 = ORIENTED_EDGE ( 'NONE', *, *, #4011, .F. ) ;
#1527 = DIRECTION ( 'NONE',  ( 0.000000000000000000, 0.000000000000000000, -1.000000000000000000 ) ) ;
#1528 = ORIENTED_EDGE ( 'NONE', *, *, #7224, .T. ) ;
#1529 = CARTESIAN_POINT ( 'NONE',  ( 34.18476129334108293, 19.96883746037050855, -259.4723857425807978 ) ) ;
#1530 = DIRECTION ( 'NONE',  ( 0.000000000000000000, 1.000000000000000000, 0.000000000000000000 ) ) ;
#1531 = CARTESIAN_POINT ( 'NONE',  ( 235.4000000000000057, 0.1024105694487990881, 5.195143123655512341 ) ) ;
#1532 = PRODUCT_DEFINITION_SHAPE ( 'NONE', 'NONE',  #13174 ) ;
#1533 = CIRCLE ( 'NONE', #7915, 230.0000000000000000 ) ;
#1534 = DIRECTION ( 'NONE',  ( 0.6368676505102707219, 0.000000000000000000, 0.7709731485165535192 ) ) ;
#1535 = FACE_BOUND ( 'NONE', #1229, .T. ) ;
#1536 = DIRECTION ( 'NONE',  ( -0.000000000000000000, -1.000000000000000000, 0.000000000000000000 ) ) ;
#1537 = DIRECTION ( 'NONE',  ( 0.3420201433256663259, 0.000000000000000000, 0.9396926207859093161 ) ) ;
#1538 = CARTESIAN_POINT ( 'NONE',  ( -229.7304253443789435, -3.777178360538905544, -11.13302378334960885 ) ) ;
#1539 = ITEM_DEFINED_TRANSFORMATION ( 'NONE', 'NONE', #10818,  #805 ) ;
#1540 = VECTOR ( 'NONE', #7162, 1000.000000000000000 ) ;
#1541 = CARTESIAN_POINT ( 'NONE',  ( -240.2963067560461923, -3.341048620459575513, -11.52705098702835684 ) ) ;
#1542 = CARTESIAN_POINT ( 'NONE',  ( 7.960204194457795477E-16, 30.00000000000000000, 201.4999999999999716 ) ) ;
#1543 = AXIS2_PLACEMENT_3D ( 'NONE', #6251, #121, #1241 ) ;
#1544 = ORIENTED_EDGE ( 'NONE', *, *, #3118, .F. ) ;
#1545 = ORIENTED_EDGE ( 'NONE', *, *, #11108, .T. ) ;
#1546 = LINE ( 'NONE', #7609, #12096 ) ;
#1547 = CARTESIAN_POINT ( 'NONE',  ( 171.3173979872628365, 20.00000000000000000, 207.3917769509529307 ) ) ;
#1548 = MANIFOLD_SOLID_BREP ( 'NONE', #2405 ) ;
#1549 = CIRCLE ( 'NONE', #6881, 248.7999999999999829 ) ;
#1550 = CARTESIAN_POINT ( 'NONE',  ( -260.7745447056980197, 20.79694577654979071, 17.06760680913495065 ) ) ;
#1551 = CARTESIAN_POINT ( 'NONE',  ( 6.337788322448691496E-13, 20.79694577634647601, -260.7745447061711275 ) ) ;
#1552 = DIRECTION ( 'NONE',  ( -0.8191520442889930198, 0.000000000000000000, 0.5735764363510443831 ) ) ;
#1553 = AXIS2_PLACEMENT_3D ( 'NONE', #8451, #1503, #4561 ) ;
#1554 = CARTESIAN_POINT ( 'NONE',  ( 222.0845275804282153, 1.749660080537334128, -0.03449061573949074866 ) ) ;
#1555 = DIRECTION ( 'NONE',  ( 0.000000000000000000, 1.000000000000000000, 0.000000000000000000 ) ) ;
#1556 = ORIENTED_EDGE ( 'NONE', *, *, #6654, .F. ) ;
#1557 = EDGE_CURVE ( 'NONE', #12455, #789, #9358, .T. ) ;
#1558 = CARTESIAN_POINT ( 'NONE',  ( 137.7829567244533564, 20.79694577634646890, -221.5672498511020194 ) ) ;
#1559 = ADVANCED_FACE ( 'NONE', ( #3226 ), #10628, .F. ) ;
#1560 = ORIENTED_EDGE ( 'NONE', *, *, #2957, .F. ) ;
#1561 = FACE_OUTER_BOUND ( 'NONE', #6989, .T. ) ;
#1562 = ORIENTED_EDGE ( 'NONE', *, *, #5129, .F. ) ;
#1563 = ORIENTED_EDGE ( 'NONE', *, *, #7436, .T. ) ;
#1564 = AXIS2_PLACEMENT_3D ( 'NONE', #769, #9821, #9893 ) ;
#1565 = VECTOR ( 'NONE', #3299, 1000.000000000000000 ) ;
#1566 = ORIENTED_EDGE ( 'NONE', *, *, #7009, .F. ) ;
#1567 = AXIS2_PLACEMENT_3D ( 'NONE', #5618, #8750, #2731 ) ;
#1568 = CARTESIAN_POINT ( 'NONE',  ( 0.000000000000000000, -13.19999999999999929, 0.000000000000000000 ) ) ;
#1569 = CARTESIAN_POINT ( 'NONE',  ( -159.9811538081799824, 20.00000000000000000, -193.6684549073582389 ) ) ;
#1570 = CIRCLE ( 'NONE', #9020, 2.000000000000000444 ) ;
#1571 = EDGE_CURVE ( 'NONE', #10870, #1370, #4875, .T. ) ;
#1572 = CARTESIAN_POINT ( 'NONE',  ( -130.5770120867059916, 20.08915143302827744, -226.1171533162815024 ) ) ;
#1573 = DIRECTION ( 'NONE',  ( -0.000000000000000000, -1.000000000000000000, 0.000000000000000000 ) ) ;
#1574 = SURFACE_STYLE_FILL_AREA ( #12504 ) ;
#1575 = AXIS2_PLACEMENT_3D ( 'NONE', #1298, #11430, #3150 ) ;
#1576 = CONTEXT_DEPENDENT_SHAPE_REPRESENTATION ( #10936, #8196 ) ;
#1577 = ORIENTED_EDGE ( 'NONE', *, *, #12335, .F. ) ;
#1578 = CARTESIAN_POINT ( 'NONE',  ( -238.7807274243665461, -0.5894492284128681758, 11.73530801150233316 ) ) ;
#1579 = ORIENTED_EDGE ( 'NONE', *, *, #8609, .T. ) ;
#1580 = CARTESIAN_POINT ( 'NONE',  ( -244.2185274279607938, 8.258776625958384798, -8.357937759674365807 ) ) ;
#1581 = EDGE_LOOP ( 'NONE', ( #11025, #11383 ) ) ;
#1582 = VECTOR ( 'NONE', #7908, 1000.000000000000000 ) ;
#1583 = DIRECTION ( 'NONE',  ( 0.000000000000000000, 0.000000000000000000, -1.000000000000000000 ) ) ;
#1584 = DIRECTION ( 'NONE',  ( -1.000000000000000000, 0.000000000000000000, 0.000000000000000000 ) ) ;
#1585 = DIRECTION ( 'NONE',  ( 0.000000000000000000, 0.000000000000000000, -1.000000000000000000 ) ) ;
#1586 = EDGE_CURVE ( 'NONE', #7801, #9902, #12304, .T. ) ;
#1587 = CARTESIAN_POINT ( 'NONE',  ( -229.8981953685927806, 9.554487809903291051, 6.849951329038304948 ) ) ;
#1588 = ADVANCED_FACE ( 'NONE', ( #9441 ), #4657, .F. ) ;
#1589 = CARTESIAN_POINT ( 'NONE',  ( 294.1869546181097235, -19.00000000000000000, 31.92980917095290749 ) ) ;
#1590 = DIRECTION ( 'NONE',  ( -0.000000000000000000, 0.01970892327970912364, 0.9998057603070482635 ) ) ;
#1591 = ITEM_DEFINED_TRANSFORMATION ( 'NONE', 'NONE', #9109,  #805 ) ;
#1592 = DIRECTION ( 'NONE',  ( 0.000000000000000000, 0.000000000000000000, 1.000000000000000000 ) ) ;
#1593 = AXIS2_PLACEMENT_3D ( 'NONE', #9413, #8353, #4338 ) ;
#1594 = ORIENTED_EDGE ( 'NONE', *, *, #9005, .T. ) ;
#1595 = ORIENTED_EDGE ( 'NONE', *, *, #3607, .T. ) ;
#1596 = CARTESIAN_POINT ( 'NONE',  ( -249.7276455222450693, -11.33491751920159452, -3.110604573866400102 ) ) ;
#1597 = ORIENTED_EDGE ( 'NONE', *, *, #7049, .T. ) ;
#1598 = CARTESIAN_POINT ( 'NONE',  ( -247.8175805190998062, 19.96883746075563693, 84.14846197946620521 ) ) ;
#1599 = CARTESIAN_POINT ( 'NONE',  ( 0.000000000000000000, 30.00000000000000000, 0.000000000000000000 ) ) ;
#1600 = DIRECTION ( 'NONE',  ( 0.000000000000000000, 1.000000000000000000, 0.000000000000000000 ) ) ;
#1601 = CARTESIAN_POINT ( 'NONE',  ( 185.9653539490014111, -19.00000000000000000, 225.1241593668316625 ) ) ;
#1602 = AXIS2_PLACEMENT_3D ( 'NONE', #6879, #5745, #6947 ) ;
#1603 = EDGE_CURVE ( 'NONE', #11485, #10920, #1237, .T. ) ;
#1604 = CARTESIAN_POINT ( 'NONE',  ( -241.2922373263966733, 5.318940986329955933, 10.75680814016106268 ) ) ;
#1605 = CARTESIAN_POINT ( 'NONE',  ( 135.8846079354933352, -30.00000000000000000, -256.1940150085812888 ) ) ;
#1606 = DIRECTION ( 'NONE',  ( -0.4162975160790937101, 0.5538822189107470706, -0.7210484489137216624 ) ) ;
#1607 = CARTESIAN_POINT ( 'NONE',  ( 229.9849294743239625, 2.311676612556695876, -2.637842061394937598 ) ) ;
#1608 = CARTESIAN_POINT ( 'NONE',  ( -248.9237871407440252, 10.19078078260020170, -5.849051582844395192 ) ) ;
#1609 = CARTESIAN_POINT ( 'NONE',  ( -241.2613930294912166, -5.271300103266470138, -10.78025408310512923 ) ) ;
#1610 = AXIS2_PLACEMENT_3D ( 'NONE', #2610, #1555, #11696 ) ;
#1611 = TOROIDAL_SURFACE ( 'NONE', #3085, 6.053020646647509828, 3.153020646647509917 ) ;
#1612 = DIRECTION ( 'NONE',  ( 0.000000000000000000, 0.000000000000000000, -1.000000000000000000 ) ) ;
#1613 = EDGE_LOOP ( 'NONE', ( #1135, #1114, #5557, #3703 ) ) ;
#1614 = VERTEX_POINT ( 'NONE', #12499 ) ;
#1615 = FACE_BOUND ( 'NONE', #10482, .T. ) ;
#1616 = CARTESIAN_POINT ( 'NONE',  ( -226.3083638767344894, 20.79694577654763421, 130.6873781513949950 ) ) ;
#1617 = CARTESIAN_POINT ( 'NONE',  ( -210.0000000000000000, 18.00000000000000000, 0.000000000000000000 ) ) ;
#1618 = DIRECTION ( 'NONE',  ( -0.9659258262890674240, 0.000000000000000000, -0.2588190451025247363 ) ) ;
#1619 = FACE_OUTER_BOUND ( 'NONE', #958, .T. ) ;
#1620 = ORIENTED_EDGE ( 'NONE', *, *, #8210, .F. ) ;
#1621 = DIRECTION ( 'NONE',  ( -0.000000000000000000, -1.000000000000000000, 0.000000000000000000 ) ) ;
#1622 = ORIENTED_EDGE ( 'NONE', *, *, #655, .T. ) ;
#1623 = EDGE_LOOP ( 'NONE', ( #874, #501, #6489, #6780 ) ) ;
#1624 = CARTESIAN_POINT ( 'NONE',  ( 171.8850263962754070, 20.08915143297735995, 196.0019244007918928 ) ) ;
#1625 = ORIENTED_EDGE ( 'NONE', *, *, #1483, .T. ) ;
#1626 = CARTESIAN_POINT ( 'NONE',  ( 0.000000000000000000, 25.00000000000000000, 0.000000000000000000 ) ) ;
#1627 = CARTESIAN_POINT ( 'NONE',  ( 0.000000000000000000, 18.00000000000000000, -196.0000000000000000 ) ) ;
#1628 = EDGE_CURVE ( 'NONE', #6909, #12286, #12124, .T. ) ;
#1629 = ADVANCED_FACE ( 'NONE', ( #8380, #12440, #3290, #7373, #91, #10207, #11148, #10141, #817, #1080, #4078, #8751, #8088, #13017, #6024 ), #9022, .F. ) ;
#1630 = CARTESIAN_POINT ( 'NONE',  ( -17.05314194221659818, 20.08915143297737416, -260.5542428351129729 ) ) ;
#1631 = CARTESIAN_POINT ( 'NONE',  ( -197.8197553893924976, 30.00000000000000000, -57.77553482998720114 ) ) ;
#1632 = DIRECTION ( 'NONE',  ( 0.000000000000000000, 0.000000000000000000, 1.000000000000000000 ) ) ;
#1633 = ORIENTED_EDGE ( 'NONE', *, *, #8745, .F. ) ;
#1634 = FACE_OUTER_BOUND ( 'NONE', #2304, .T. ) ;
#1635 = VERTEX_POINT ( 'NONE', #6954 ) ;
#1636 = PRODUCT_DEFINITION_SHAPE ( 'NONE', 'NONE',  #13166 ) ;
#1637 = CARTESIAN_POINT ( 'NONE',  ( -241.3417439075342656, 5.375691555194026527, -10.44818116087475879 ) ) ;
#1638 = ORIENTED_EDGE ( 'NONE', *, *, #12741, .T. ) ;
#1639 = CARTESIAN_POINT ( 'NONE',  ( -221.6213872890270977, -29.00000000000000000, 190.2057062658400923 ) ) ;
#1640 = FACE_OUTER_BOUND ( 'NONE', #10969, .T. ) ;
#1641 = DIRECTION ( 'NONE',  ( -0.000000000000000000, -1.000000000000000000, 0.000000000000000000 ) ) ;
#1642 = CARTESIAN_POINT ( 'NONE',  ( 0.000000000000000000, -19.00000000000000000, 0.000000000000000000 ) ) ;
#1643 = PRODUCT_DEFINITION_SHAPE ( 'NONE', 'NONE',  #13122 ) ;
#1644 = CARTESIAN_POINT ( 'NONE',  ( -245.5963909204522224, -9.039317601314641237, 7.892311131002199609 ) ) ;
#1645 = AXIS2_PLACEMENT_3D ( 'NONE', #2829, #7776, #7980 ) ;
#1646 = CARTESIAN_POINT ( 'NONE',  ( -210.0000000000000000, 19.40000000000000213, 5.100000000000000533 ) ) ;
#1647 =( REPRESENTATION_RELATIONSHIP ('NONE','NONE', #12019, #182 ) REPRESENTATION_RELATIONSHIP_WITH_TRANSFORMATION ( #5569 )SHAPE_REPRESENTATION_RELATIONSHIP( ) );
#1648 = VERTEX_POINT ( 'NONE', #5141 ) ;
#1649 = CARTESIAN_POINT ( 'NONE',  ( -229.7197234876223888, 3.908141881471038026, 11.35191153251636820 ) ) ;
#1650 = CONTEXT_DEPENDENT_SHAPE_REPRESENTATION ( #173, #3141 ) ;
#1651 = EDGE_LOOP ( 'NONE', ( #9963, #7430, #3042, #2675 ) ) ;
#1652 = ADVANCED_FACE ( 'NONE', ( #9945, #11211 ), #2077, .F. ) ;
#1653 = ORIENTED_EDGE ( 'NONE', *, *, #8666, .T. ) ;
#1654 = ADVANCED_FACE ( 'NONE', ( #954 ), #8954, .F. ) ;
#1655 = CARTESIAN_POINT ( 'NONE',  ( -249.7806011017298715, -11.58204051041879801, -1.980500725180536659 ) ) ;
#1656 = ORIENTED_EDGE ( 'NONE', *, *, #6531, .F. ) ;
#1657 =( GEOMETRIC_REPRESENTATION_CONTEXT ( 3 ) GLOBAL_UNCERTAINTY_ASSIGNED_CONTEXT ( ( #4882 ) ) GLOBAL_UNIT_ASSIGNED_CONTEXT ( ( #2562, #6643, #5635 ) ) REPRESENTATION_CONTEXT ( 'NONE', 'WORKASPACE' ) );
#1658 = CARTESIAN_POINT ( 'NONE',  ( -207.7919029851962023, 20.55460285100346596, -159.4136521840017906 ) ) ;
#1659 = DIRECTION ( 'NONE',  ( 0.6368676505102716101, 0.000000000000000000, 0.7709731485165527420 ) ) ;
#1660 = DIRECTION ( 'NONE',  ( 0.000000000000000000, -0.01970892327970899874, -0.9998057603070481525 ) ) ;
#1661 = DIRECTION ( 'NONE',  ( -0.4503334343941627904, -0.7071067811865381358, -0.5451603414288054283 ) ) ;
#1662 = CARTESIAN_POINT ( 'NONE',  ( -290.6841825403030839, -30.00000000000000000, -27.68945685411394919 ) ) ;
#1663 = DIRECTION ( 'NONE',  ( 0.000000000000000000, 0.9998057603070481525, -0.01970892327970899874 ) ) ;
#1664 = DIRECTION ( 'NONE',  ( -0.8191520442889949072, 0.000000000000000000, 0.5735764363510416075 ) ) ;
#1665 = CARTESIAN_POINT ( 'NONE',  ( -229.9415104875559734, -10.54483369259275349, -5.197775207300905365 ) ) ;
#1666 = CONTEXT_DEPENDENT_SHAPE_REPRESENTATION ( #10582, #3663 ) ;
#1667 = AXIS2_PLACEMENT_3D ( 'NONE', #2730, #6821, #5820 ) ;
#1668 = CARTESIAN_POINT ( 'NONE',  ( -248.8244828231558472, 10.12360735459614602, -5.964490512238578290 ) ) ;
#1669 = DIRECTION ( 'NONE',  ( 0.000000000000000000, 0.000000000000000000, -1.000000000000000000 ) ) ;
#1670 = EDGE_CURVE ( 'NONE', #2427, #8254, #1884, .T. ) ;
#1671 = CARTESIAN_POINT ( 'NONE',  ( -229.7894208366921021, -6.875096941970043396, -9.842338683517198206 ) ) ;
#1672 = ORIENTED_EDGE ( 'NONE', *, *, #4894, .F. ) ;
#1673 = EDGE_LOOP ( 'NONE', ( #4388, #2858 ) ) ;
#1674 = CARTESIAN_POINT ( 'NONE',  ( 0.000000000000000000, 30.00000000000000000, -202.4999999999999716 ) ) ;
#1675 = DIRECTION ( 'NONE',  ( 0.000000000000000000, 1.000000000000000000, 0.000000000000000000 ) ) ;
#1676 = AXIS2_PLACEMENT_3D ( 'NONE', #6963, #8111, #8096 ) ;
#1677 = PRODUCT_DEFINITION_SHAPE ( 'NONE', 'NONE',  #13066 ) ;
#1678 = EDGE_CURVE ( 'NONE', #10191, #5629, #203, .T. ) ;
#1679 = AXIS2_PLACEMENT_3D ( 'NONE', #1125, #8059, #931 ) ;
#1680 = CIRCLE ( 'NONE', #1258, 2.500000000000025313 ) ;
#1681 = CARTESIAN_POINT ( 'NONE',  ( -247.4557548097905055, 20.79694577642381859, 84.02568524162670371 ) ) ;
#1682 = AXIS2_PLACEMENT_3D ( 'NONE', #4014, #6899, #9951 ) ;
#1683 = CARTESIAN_POINT ( 'NONE',  ( -240.0143494547951377, -2.418590316237056115, -11.50416929261772303 ) ) ;
#1684 = DIRECTION ( 'NONE',  ( 0.08715574274766503537, 0.000000000000000000, -0.9961946980917451011 ) ) ;
#1685 = CARTESIAN_POINT ( 'NONE',  ( 0.000000000000000000, -20.00000000000000000, 0.000000000000000000 ) ) ;
#1686 = CARTESIAN_POINT ( 'NONE',  ( 240.1560849993289537, 2.274296953688199618, -2.660406300278597591 ) ) ;
#1687 = CONICAL_SURFACE ( 'NONE', #7433, 6.500000000000005329, 0.7853981633974476129 ) ;
#1688 = EDGE_LOOP ( 'NONE', ( #1790, #6635, #590, #6451, #1919, #7286 ) ) ;
#1689 = AXIS2_PLACEMENT_3D ( 'NONE', #11529, #5578, #3440 ) ;
#1690 = DIRECTION ( 'NONE',  ( 0.000000000000000000, 1.000000000000000000, 0.000000000000000000 ) ) ;
#1691 = VERTEX_POINT ( 'NONE', #5891 ) ;
#1692 = ORIENTED_EDGE ( 'NONE', *, *, #2881, .T. ) ;
#1693 = CARTESIAN_POINT ( 'NONE',  ( 233.8077470125390676, 20.08915143297735995, 115.3046144132253943 ) ) ;
#1694 = ORIENTED_EDGE ( 'NONE', *, *, #2415, .F. ) ;
#1695 = AXIS2_PLACEMENT_3D ( 'NONE', #8157, #5070, #4881 ) ;
#1696 = CARTESIAN_POINT ( 'NONE',  ( 130.7196491263533460, -20.69999999999999929, -200.0834159351620940 ) ) ;
#1697 = CARTESIAN_POINT ( 'NONE',  ( 238.9791647118778144, -0.1781744853868436618, -3.496576182273237077 ) ) ;
#1698 = CARTESIAN_POINT ( 'NONE',  ( 212.6409525001303962, -22.00000000000000000, 138.9238112054132159 ) ) ;
#1699 = TOROIDAL_SURFACE ( 'NONE', #12760, 250.0000000000000000, 10.00000000000000000 ) ;
#1700 = LINE ( 'NONE', #9958, #3917 ) ;
#1701 = CARTESIAN_POINT ( 'NONE',  ( -247.9656915555145815, 9.808762669553802382, 6.469331566347206852 ) ) ;
#1702 = VECTOR ( 'NONE', #8523, 1000.000000000000000 ) ;
#1703 = VERTEX_POINT ( 'NONE', #3881 ) ;
#1704 = CARTESIAN_POINT ( 'NONE',  ( 3.056106087272219914E-14, 25.00000000000000000, -249.2999999999999829 ) ) ;
#1705 = ORIENTED_EDGE ( 'NONE', *, *, #3097, .F. ) ;
#1706 = CARTESIAN_POINT ( 'NONE',  ( -243.1580368188211310, 7.448595192303357315, -9.087405006429683851 ) ) ;
#1707 = VERTEX_POINT ( 'NONE', #5956 ) ;
#1708 = EDGE_CURVE ( 'NONE', #497, #7072, #7645, .T. ) ;
#1709 = CIRCLE ( 'NONE', #4673, 5.500000000000015099 ) ;
#1710 = CARTESIAN_POINT ( 'NONE',  ( 0.000000000000000000, 21.94174202707280941, 0.000000000000000000 ) ) ;
#1711 = AXIS2_PLACEMENT_3D ( 'NONE', #4928, #9001, #11740 ) ;
#1712 = FACE_OUTER_BOUND ( 'NONE', #7058, .T. ) ;
#1713 = DIRECTION ( 'NONE',  ( -0.000000000000000000, 1.000000000000000000, 0.000000000000000000 ) ) ;
#1714 = CARTESIAN_POINT ( 'NONE',  ( -229.8895716818989285, 9.351917924694065576, -7.154906690919313306 ) ) ;
#1715 = VECTOR ( 'NONE', #9476, 1000.000000000000114 ) ;
#1716 = CARTESIAN_POINT ( 'NONE',  ( -245.1341653186248379, -8.810613775770821832, 8.147076446021827678 ) ) ;
#1717 = CARTESIAN_POINT ( 'NONE',  ( -238.6985546661037176, 0.1084670113012983633, -12.00000001867801913 ) ) ;
#1718 = CONTEXT_DEPENDENT_SHAPE_REPRESENTATION ( #5483, #1177 ) ;
#1719 = ORIENTED_EDGE ( 'NONE', *, *, #9961, .T. ) ;
#1720 = DIRECTION ( 'NONE',  ( 0.000000000000000000, 0.000000000000000000, 1.000000000000000000 ) ) ;
#1721 = DIRECTION ( 'NONE',  ( 0.000000000000000000, 0.000000000000000000, -1.000000000000000000 ) ) ;
#1722 = ORIENTED_EDGE ( 'NONE', *, *, #12793, .T. ) ;
#1723 = EDGE_CURVE ( 'NONE', #11697, #10031, #10016, .T. ) ;
#1724 = EDGE_CURVE ( 'NONE', #497, #1707, #4946, .T. ) ;
#1725 = VERTEX_POINT ( 'NONE', #1951 ) ;
#1726 = CARTESIAN_POINT ( 'NONE',  ( -249.4468820693415410, -10.72473316041474334, -4.809560399683298293 ) ) ;
#1727 = EDGE_LOOP ( 'NONE', ( #12687, #9600, #8517, #4341 ) ) ;
#1728 = CARTESIAN_POINT ( 'NONE',  ( -252.9796497735838443, 20.55460285104794949, 67.76049180365761515 ) ) ;
#1729 = CARTESIAN_POINT ( 'NONE',  ( -210.0000000000000000, 19.40000000000000213, 0.000000000000000000 ) ) ;
#1730 = DIRECTION ( 'NONE',  ( -0.000000000000000000, -1.000000000000000000, 0.000000000000000000 ) ) ;
#1731 = FACE_OUTER_BOUND ( 'NONE', #10353, .T. ) ;
#1732 = AXIS2_PLACEMENT_3D ( 'NONE', #4628, #9767, #1448 ) ;
#1733 = FILL_AREA_STYLE ('',( #5030 ) ) ;
#1734 = DIRECTION ( 'NONE',  ( -0.6368676505102698338, 0.000000000000000000, -0.7709731485165541853 ) ) ;
#1735 = EDGE_CURVE ( 'NONE', #7894, #5758, #7229, .T. ) ;
#1736 = DIRECTION ( 'NONE',  ( 0.4503334343941626794, -0.7071067811865380248, 0.5451603414288055394 ) ) ;
#1737 = DIRECTION ( 'NONE',  ( -0.8660254037844345998, 0.000000000000000000, -0.5000000000000071054 ) ) ;
#1738 = CARTESIAN_POINT ( 'NONE',  ( 229.9733680233430277, 0.4624089970348260192, 3.499999999999964917 ) ) ;
#1739 = VECTOR ( 'NONE', #3289, 1000.000000000000000 ) ;
#1740 = CARTESIAN_POINT ( 'NONE',  ( -249.7266004383521079, 11.33448610545603685, -3.100135285984364053 ) ) ;
#1741 = CARTESIAN_POINT ( 'NONE',  ( 138.9238112054132159, -22.00000000000000000, -212.6409525001303962 ) ) ;
#1742 = EDGE_CURVE ( 'NONE', #1954, #10191, #6558, .T. ) ;
#1743 = CARTESIAN_POINT ( 'NONE',  ( 235.4000000000000057, -4.447920636657316074, 2.686261716586446635 ) ) ;
#1744 = ORIENTED_EDGE ( 'NONE', *, *, #7425, .F. ) ;
#1745 = EDGE_LOOP ( 'NONE', ( #4372, #10086 ) ) ;
#1746 = DIRECTION ( 'NONE',  ( 8.659560562354963673E-17, 0.7071067811865450192, -0.7071067811865500152 ) ) ;
#1747 = FACE_BOUND ( 'NONE', #7385, .T. ) ;
#1748 = ADVANCED_FACE ( 'NONE', ( #12150 ), #12548, .T. ) ;
#1749 = CARTESIAN_POINT ( 'NONE',  ( 247.9906035362907915, 20.55460285157398914, 84.20717312406510757 ) ) ;
#1750 = EDGE_CURVE ( 'NONE', #1635, #12270, #7019, .T. ) ;
#1751 = DIRECTION ( 'NONE',  ( 0.6368676505102716101, 0.000000000000000000, 0.7709731485165527420 ) ) ;
#1752 = DIRECTION ( 'NONE',  ( -0.2588190451025145777, 0.000000000000000000, -0.9659258262890699775 ) ) ;
#1753 = DIRECTION ( 'NONE',  ( 0.000000000000000000, 0.000000000000000000, 1.000000000000000000 ) ) ;
#1754 = AXIS2_PLACEMENT_3D ( 'NONE', #1307, #8638, #7507 ) ;
#1755 = CARTESIAN_POINT ( 'NONE',  ( -286.5648042451072115, -19.40000000000000213, 14.34944810630078393 ) ) ;
#1756 = ORIENTED_EDGE ( 'NONE', *, *, #2125, .T. ) ;
#1757 = CIRCLE ( 'NONE', #1543, 5.500000000000005329 ) ;
#1758 = EDGE_CURVE ( 'NONE', #169, #11069, #11704, .T. ) ;
#1759 = CARTESIAN_POINT ( 'NONE',  ( -238.6985546649171397, -0.2132982402979453351, 12.00000003664865922 ) ) ;
#1760 = VERTEX_POINT ( 'NONE', #7155 ) ;
#1761 = ORIENTED_EDGE ( 'NONE', *, *, #11687, .T. ) ;
#1762 = CARTESIAN_POINT ( 'NONE',  ( 239.8763759935506528, -1.918973793115196225, 2.928207549569424195 ) ) ;
#1763 = ORIENTED_EDGE ( 'NONE', *, *, #9005, .F. ) ;
#1764 = PRODUCT_DEFINITION_SHAPE ( 'NONE', 'NONE',  #13108 ) ;
#1765 = CIRCLE ( 'NONE', #11335, 250.1999999999999602 ) ;
#1766 = CARTESIAN_POINT ( 'NONE',  ( 0.000000000000000000, -20.00000000000000000, 248.7999999999999829 ) ) ;
#1767 = AXIS2_PLACEMENT_3D ( 'NONE', #5566, #3355, #7441 ) ;
#1768 = CARTESIAN_POINT ( 'NONE',  ( -234.1947771728870009, 20.08915143306511553, -115.4648407706533959 ) ) ;
#1769 = EDGE_CURVE ( 'NONE', #9162, #1505, #1905, .T. ) ;
#1770 = FACE_OUTER_BOUND ( 'NONE', #2245, .T. ) ;
#1771 =( NAMED_UNIT ( * ) SI_UNIT ( $, .STERADIAN. ) SOLID_ANGLE_UNIT ( ) );
#1772 = DIRECTION ( 'NONE',  ( 0.4503334343941562956, -0.7071067811865480168, 0.5451603414287978788 ) ) ;
#1773 = ORIENTED_EDGE ( 'NONE', *, *, #7779, .T. ) ;
#1774 = CARTESIAN_POINT ( 'NONE',  ( 2.400307726328812059E-14, 18.00000000000000000, 196.0000000000000000 ) ) ;
#1775 = CIRCLE ( 'NONE', #4735, 2.000000000000000444 ) ;
#1776 = ORIENTED_EDGE ( 'NONE', *, *, #4487, .F. ) ;
#1777 = VECTOR ( 'NONE', #3678, 1000.000000000000000 ) ;
#1778 = CARTESIAN_POINT ( 'NONE',  ( -245.3834146146978981, 8.931379171135056083, -7.634986101342768450 ) ) ;
#1779 = ORIENTED_EDGE ( 'NONE', *, *, #1434, .F. ) ;
#1780 = CLOSED_SHELL ( 'NONE', ( #12899, #2477, #4181, #9023, #10038, #1277, #3197, #1559, #10098, #7265, #4414, #11203, #10056 ) ) ;
#1781 = AXIS2_PLACEMENT_3D ( 'NONE', #3671, #5814, #5882 ) ;
#1782 = DIRECTION ( 'NONE',  ( 1.000000000000000000, 0.000000000000000000, 0.000000000000000000 ) ) ;
#1783 = CARTESIAN_POINT ( 'NONE',  ( -249.7379166007395384, -10.64944549071737612, -5.654815128212893782 ) ) ;
#1784 = CARTESIAN_POINT ( 'NONE',  ( -229.7150392099732414, 2.684421947324201252, -11.44580934118247662 ) ) ;
#1785 = AXIS2_PLACEMENT_3D ( 'NONE', #3701, #10704, #8643 ) ;
#1786 = CARTESIAN_POINT ( 'NONE',  ( -211.9058003148610112, 20.08915143297736705, 151.8458048843639858 ) ) ;
#1787 = VECTOR ( 'NONE', #343, 1000.000000000000000 ) ;
#1788 = CARTESIAN_POINT ( 'NONE',  ( -244.0248830888179725, -8.135989420001664030, 8.821260460492251099 ) ) ;
#1789 = CARTESIAN_POINT ( 'NONE',  ( 6.337788322448691496E-13, 20.79694577634647601, -260.7745447061711275 ) ) ;
#1790 = ORIENTED_EDGE ( 'NONE', *, *, #8838, .F. ) ;
#1791 = DIRECTION ( 'NONE',  ( 0.000000000000000000, 1.000000000000000000, 0.000000000000000000 ) ) ;
#1792 = ORIENTED_EDGE ( 'NONE', *, *, #6213, .F. ) ;
#1793 = PRODUCT_DEFINITION_SHAPE ( 'NONE', 'NONE',  #12069 ) ;
#1794 = AXIS2_PLACEMENT_3D ( 'NONE', #8969, #7970, #1096 ) ;
#1795 = ORIENTED_EDGE ( 'NONE', *, *, #8602, .T. ) ;
#1796 = CARTESIAN_POINT ( 'NONE',  ( -249.7621493473840815, -11.48044694427989931, -2.508021710844266394 ) ) ;
#1797 = ORIENTED_EDGE ( 'NONE', *, *, #7193, .F. ) ;
#1798 = CARTESIAN_POINT ( 'NONE',  ( -196.8887528224093444, 20.55460285074426707, 172.6991790975775132 ) ) ;
#1799 = CARTESIAN_POINT ( 'NONE',  ( -210.0000000000000000, 30.00000000000000000, 0.000000000000000000 ) ) ;
#1800 = LINE ( 'NONE', #7724, #9130 ) ;
#1801 = AXIS2_PLACEMENT_3D ( 'NONE', #3853, #3046, #7061 ) ;
#1802 = CARTESIAN_POINT ( 'NONE',  ( -197.8197553893909912, 29.00000000000000000, 64.27553482999130097 ) ) ;
#1803 = ADVANCED_FACE ( 'NONE', ( #9351 ), #6808, .F. ) ;
#1804 = FACE_OUTER_BOUND ( 'NONE', #7248, .T. ) ;
#1805 = EDGE_CURVE ( 'NONE', #1707, #6121, #10843, .T. ) ;
#1806 = AXIS2_PLACEMENT_3D ( 'NONE', #5372, #510, #8449 ) ;
#1807 = AXIS2_PLACEMENT_3D ( 'NONE', #10386, #9396, #11401 ) ;
#1808 = DIRECTION ( 'NONE',  ( -0.9396926207859058744, 0.000000000000000000, -0.3420201433256757628 ) ) ;
#1809 = CARTESIAN_POINT ( 'NONE',  ( -229.7747724777948122, -5.884216672786659608, 10.17777400990889447 ) ) ;
#1810 = CONTEXT_DEPENDENT_SHAPE_REPRESENTATION ( #9478, #5692 ) ;
#1811 = B_SPLINE_CURVE_WITH_KNOTS ( 'NONE', 3,
 ( #2323, #6401, #8402, #263, #1130, #7330, #6468, #10459, #5457, #12462, #1263, #4321, #2258, #8530, #3315, #7393, #4447, #1330, #10525, #1397, #12590, #9518, #8269, #11261, #5188, #3185, #527, #7784, #11662, #4778, #7587, #7715, #1523, #8596, #12849, #2516, #10721, #5587, #9647, #4576, #10585, #8720, #8656, #5522, #1453, #6663, #2454, #7527, #6731, #3716, #8854, #11854, #12713, #3578, #9775, #728, #10781, #11795, #7649, #6530, #1649, #10847, #5788, #3447, #4708 ),
 .UNSPECIFIED., .F., .F.,
 ( 4, 2, 2, 2, 2, 2, 2, 2, 2, 2, 2, 2, 2, 2, 1, 2, 2, 2, 2, 2, 2, 2, 1, 2, 2, 1, 2, 2, 2, 2, 2, 2, 2, 4 ),
 ( 0.000000000000000000, 0.03125000000000011102, 0.06250000000000022204, 0.09375000000000036082, 0.1093750000000003886, 0.1250000000000004163, 0.1562500000000004718, 0.1875000000000005274, 0.2187500000000005829, 0.2500000000000006661, 0.3125000000000008882, 0.3750000000000011102, 0.4062500000000012212, 0.4375000000000013323, 0.4687500000000013878, 0.4843750000000014433, 0.5000000000000014433, 0.5625000000000016653, 0.5937500000000017764, 0.6250000000000018874, 0.6562500000000019984, 0.6875000000000021094, 0.7187500000000022204, 0.7343750000000021094, 0.7500000000000021094, 0.7812500000000018874, 0.7968750000000016653, 0.8125000000000015543, 0.8437500000000012212, 0.8593750000000009992, 0.8750000000000008882, 0.9062500000000006661, 0.9375000000000004441, 1.000000000000000000 ),
 .UNSPECIFIED. ) ;
#1812 = CARTESIAN_POINT ( 'NONE',  ( -249.7095932329616517, 11.27773618852464743, -3.298468580809413186 ) ) ;
#1813 = CARTESIAN_POINT ( 'NONE',  ( -229.8369385731911905, -8.312474322141341077, -8.662778311384863983 ) ) ;
#1814 = ORIENTED_EDGE ( 'NONE', *, *, #9154, .F. ) ;
#1815 = EDGE_LOOP ( 'NONE', ( #5492, #1887 ) ) ;
#1816 = CARTESIAN_POINT ( 'NONE',  ( 192.8974817588416784, -30.00000000000000000, -159.3442861576696998 ) ) ;
#1817 = CARTESIAN_POINT ( 'NONE',  ( -252.4341100429120104, 20.79694577648844245, 67.61424743034129392 ) ) ;
#1818 = FACE_OUTER_BOUND ( 'NONE', #12368, .T. ) ;
#1819 = DIRECTION ( 'NONE',  ( 0.3420201433256757628, 0.000000000000000000, -0.9396926207859058744 ) ) ;
#1820 = CYLINDRICAL_SURFACE ( 'NONE', #1832, 250.1999999999999602 ) ;
#1821 = ORIENTED_EDGE ( 'NONE', *, *, #5754, .F. ) ;
#1822 = AXIS2_PLACEMENT_3D ( 'NONE', #11165, #6104, #10155 ) ;
#1823 = DIRECTION ( 'NONE',  ( 1.000000000000000000, -0.000000000000000000, 1.224646799147353207E-16 ) ) ;
#1824 = UNCERTAINTY_MEASURE_WITH_UNIT (LENGTH_MEASURE( 1.000000000000000082E-05 ), #12896, 'distance_accuracy_value', 'NONE');
#1825 = CARTESIAN_POINT ( 'NONE',  ( -239.4909294218351761, -1.818763037284782724, 11.86135881504065992 ) ) ;
#1826 = ORIENTED_EDGE ( 'NONE', *, *, #428, .F. ) ;
#1827 = EDGE_LOOP ( 'NONE', ( #6840, #4915 ) ) ;
#1828 = EDGE_CURVE ( 'NONE', #6569, #4077, #6592, .T. ) ;
#1829 = EDGE_CURVE ( 'NONE', #3502, #1020, #7408, .T. ) ;
#1830 = DIRECTION ( 'NONE',  ( 0.000000000000000000, 0.000000000000000000, 1.000000000000000000 ) ) ;
#1831 = EDGE_LOOP ( 'NONE', ( #11112, #1756, #1653 ) ) ;
#1832 = AXIS2_PLACEMENT_3D ( 'NONE', #5888, #814, #4877 ) ;
#1833 = CARTESIAN_POINT ( 'NONE',  ( 71.82423009839129691, 30.00000000000000000, -197.3354503650404865 ) ) ;
#1834 = APPLICATION_CONTEXT ( 'automotive_design' ) ;
#1835 = CARTESIAN_POINT ( 'NONE',  ( -67.55708173888510260, 20.08915143292433214, 252.2208631666720180 ) ) ;
#1836 = AXIS2_PLACEMENT_3D ( 'NONE', #10262, #12, #4937 ) ;
#1837 = DIRECTION ( 'NONE',  ( 0.000000000000000000, 1.000000000000000000, 0.000000000000000000 ) ) ;
#1838 = CARTESIAN_POINT ( 'NONE',  ( -233.0000000000000000, 0.000000000000000000, 0.000000000000000000 ) ) ;
#1839 = ORIENTED_EDGE ( 'NONE', *, *, #370, .T. ) ;
#1840 = DIRECTION ( 'NONE',  ( 0.000000000000000000, 0.000000000000000000, -1.000000000000000000 ) ) ;
#1841 = EDGE_LOOP ( 'NONE', ( #2251, #12872 ) ) ;
#1842 = CARTESIAN_POINT ( 'NONE',  ( -239.0190678720388178, 1.196910331790569160, 11.68891451185957031 ) ) ;
#1843 = EDGE_LOOP ( 'NONE', ( #3886, #8579, #654, #10406 ) ) ;
#1844 = ADVANCED_FACE ( 'NONE', ( #10276 ), #6418, .F. ) ;
#1845 =( REPRESENTATION_RELATIONSHIP ('NONE','NONE', #12019, #182 ) REPRESENTATION_RELATIONSHIP_WITH_TRANSFORMATION ( #9349 )SHAPE_REPRESENTATION_RELATIONSHIP( ) );
#1846 = CARTESIAN_POINT ( 'NONE',  ( 240.2035656452229091, -2.353769564549843984, -2.590352657762025501 ) ) ;
#1847 = CARTESIAN_POINT ( 'NONE',  ( 0.000000000000000000, 24.75600756274008063, 0.000000000000000000 ) ) ;
#1848 = FACE_OUTER_BOUND ( 'NONE', #8984, .T. ) ;
#1849 = CYLINDRICAL_SURFACE ( 'NONE', #8470, 8.000000000000007105 ) ;
#1850 = EDGE_CURVE ( 'NONE', #7200, #2165, #8357, .T. ) ;
#1851 = FACE_BOUND ( 'NONE', #4535, .T. ) ;
#1852 = CARTESIAN_POINT ( 'NONE',  ( -241.3214569865913006, -5.363580936720061310, 10.73461844913211216 ) ) ;
#1853 = CARTESIAN_POINT ( 'NONE',  ( -178.3611219674583310, 20.79694577634646535, -190.4297758776780256 ) ) ;
#1854 = UNCERTAINTY_MEASURE_WITH_UNIT (LENGTH_MEASURE( 1.000000000000000082E-05 ), #3560, 'distance_accuracy_value', 'NONE');
#1855 = EDGE_LOOP ( 'NONE', ( #6438, #8683, #1233, #4846 ) ) ;
#1856 = CARTESIAN_POINT ( 'NONE',  ( -238.8528738665295350, -0.8456521594436280376, -11.72073125521067638 ) ) ;
#1857 = ORIENTED_EDGE ( 'NONE', *, *, #9342, .F. ) ;
#1858 = VERTEX_POINT ( 'NONE', #6222 ) ;
#1859 = CIRCLE ( 'NONE', #10578, 5.500000000000015099 ) ;
#1860 = CARTESIAN_POINT ( 'NONE',  ( -249.3654635700585800, -10.61071050137281091, -5.052935793542020271 ) ) ;
#1861 = ORIENTED_EDGE ( 'NONE', *, *, #9054, .F. ) ;
#1862 = CARTESIAN_POINT ( 'NONE',  ( 67.76049180280260487, 20.55460285165543155, -252.9796497734500917 ) ) ;
#1863 = CARTESIAN_POINT ( 'NONE',  ( -210.0000000000000000, 19.40000000000000213, 0.000000000000000000 ) ) ;
#1864 = CARTESIAN_POINT ( 'NONE',  ( 0.000000000000000000, 18.00000000000000000, -208.0000000000000000 ) ) ;
#1865 = DIRECTION ( 'NONE',  ( -0.4503334343941556295, 0.7071067811865489050, -0.5451603414287969906 ) ) ;
#1866 = AXIS2_PLACEMENT_3D ( 'NONE', #7709, #5710, #9769 ) ;
#1867 = CARTESIAN_POINT ( 'NONE',  ( -249.7915528516602990, 11.82778639354381767, 2.343958593093920850 ) ) ;
#1868 = DIRECTION ( 'NONE',  ( -0.9848077530122067991, 0.000000000000000000, -0.1736481776669374644 ) ) ;
#1869 = DIRECTION ( 'NONE',  ( 0.6368676505102696117, 0.000000000000000000, 0.7709731485165545184 ) ) ;
#1870 = PRODUCT_DEFINITION_SHAPE ( 'NONE', 'NONE',  #13162 ) ;
#1871 = CARTESIAN_POINT ( 'NONE',  ( -160.3845033201291130, -9.830508068730530624, -194.1567379013694392 ) ) ;
#1872 = VERTEX_POINT ( 'NONE', #286 ) ;
#1873 = ORIENTED_EDGE ( 'NONE', *, *, #12559, .T. ) ;
#1874 = EDGE_CURVE ( 'NONE', #2184, #6551, #5763, .T. ) ;
#1875 = CARTESIAN_POINT ( 'NONE',  ( -0.000000000000000000, -19.00000000000000000, 0.000000000000000000 ) ) ;
#1876 = DIRECTION ( 'NONE',  ( 0.000000000000000000, -0.8757116489157734662, -0.4828344519120573719 ) ) ;
#1877 = FACE_OUTER_BOUND ( 'NONE', #6763, .T. ) ;
#1878 = AXIS2_PLACEMENT_3D ( 'NONE', #3875, #10877, #9807 ) ;
#1879 = DIRECTION ( 'NONE',  ( 0.000000000000000000, -1.000000000000000000, 0.000000000000000000 ) ) ;
#1880 = DIRECTION ( 'NONE',  ( 0.7071067811865536790, 0.000000000000000000, -0.7071067811865413555 ) ) ;
#1881 = CARTESIAN_POINT ( 'NONE',  ( -245.3956592408875395, -8.937419274662552482, 7.627912038472048906 ) ) ;
#1882 = ITEM_DEFINED_TRANSFORMATION ( 'NONE', 'NONE', #4632,  #805 ) ;
#1883 = ORIENTED_EDGE ( 'NONE', *, *, #7660, .F. ) ;
#1884 = LINE ( 'NONE', #3073, #2535 ) ;
#1885 = AXIS2_PLACEMENT_3D ( 'NONE', #6029, #5018, #6159 ) ;
#1886 = CARTESIAN_POINT ( 'NONE',  ( -122.2593324768321992, 30.00000000000000000, 161.7755348299905052 ) ) ;
#1887 = ORIENTED_EDGE ( 'NONE', *, *, #7545, .T. ) ;
#1888 = AXIS2_PLACEMENT_3D ( 'NONE', #9686, #2619, #830 ) ;
#1889 = ORIENTED_EDGE ( 'NONE', *, *, #7552, .T. ) ;
#1890 = CIRCLE ( 'NONE', #2310, 5.500000000000005329 ) ;
#1891 = LINE ( 'NONE', #8094, #8068 ) ;
#1892 = ORIENTED_EDGE ( 'NONE', *, *, #10963, .T. ) ;
#1893 = VECTOR ( 'NONE', #4417, 1000.000000000000227 ) ;
#1894 = CARTESIAN_POINT ( 'NONE',  ( -248.5901226953540402, 9.992747119206066841, 6.181484274903534804 ) ) ;
#1895 = CIRCLE ( 'NONE', #7006, 5.100000000000000533 ) ;
#1896 = CARTESIAN_POINT ( 'NONE',  ( 207.1687172321464914, 20.08915143279739013, 158.9353507257995091 ) ) ;
#1897 = CARTESIAN_POINT ( 'NONE',  ( -0.000000000000000000, -29.00000000000000000, 0.000000000000000000 ) ) ;
#1898 =( NAMED_UNIT ( * ) SI_UNIT ( $, .STERADIAN. ) SOLID_ANGLE_UNIT ( ) );
#1899 = EDGE_CURVE ( 'NONE', #9833, #157, #448, .T. ) ;
#1900 = AXIS2_PLACEMENT_3D ( 'NONE', #7905, #11788, #10776 ) ;
#1901 = EDGE_CURVE ( 'NONE', #10068, #9249, #11935, .T. ) ;
#1902 = ORIENTED_EDGE ( 'NONE', *, *, #2369, .T. ) ;
#1903 = DIRECTION ( 'NONE',  ( 0.000000000000000000, 0.000000000000000000, 1.000000000000000000 ) ) ;
#1904 = VERTEX_POINT ( 'NONE', #8420 ) ;
#1905 = CIRCLE ( 'NONE', #12756, 5.099999999999993427 ) ;
#1906 = FACE_OUTER_BOUND ( 'NONE', #640, .T. ) ;
#1907 = EDGE_LOOP ( 'NONE', ( #12689, #8704, #2989, #589 ) ) ;
#1908 = CONICAL_SURFACE ( 'NONE', #4044, 5.500000000000005329, 0.7853981633974461696 ) ;
#1909 = CARTESIAN_POINT ( 'NONE',  ( -251.0000000000000000, 22.00000000000000000, 0.000000000000000000 ) ) ;
#1910 = CARTESIAN_POINT ( 'NONE',  ( 240.1928509381578465, 2.335100009138994182, 2.607195044851006394 ) ) ;
#1911 = FACE_OUTER_BOUND ( 'NONE', #7471, .T. ) ;
#1912 = CARTESIAN_POINT ( 'NONE',  ( -229.7584495954988881, 5.207945372205803558, -10.53982534208329191 ) ) ;
#1913 = LINE ( 'NONE', #4039, #11378 ) ;
#1914 = CARTESIAN_POINT ( 'NONE',  ( -244.8216528716611435, -8.638952368812793381, 8.328775922993848724 ) ) ;
#1915 = ADVANCED_FACE ( 'NONE', ( #2272 ), #651, .F. ) ;
#1916 = EDGE_CURVE ( 'NONE', #5028, #10886, #3317, .T. ) ;
#1917 = CARTESIAN_POINT ( 'NONE',  ( -137.7829567244531006, 20.79694577634646535, -221.5672498511021615 ) ) ;
#1918 = ITEM_DEFINED_TRANSFORMATION ( 'NONE', 'NONE', #6349,  #805 ) ;
#1919 = ORIENTED_EDGE ( 'NONE', *, *, #5637, .F. ) ;
#1920 = CARTESIAN_POINT ( 'NONE',  ( -238.9443119694662414, -1.049071734835953063, -11.70307552047284894 ) ) ;
#1921 = VERTEX_POINT ( 'NONE', #4462 ) ;
#1922 = ADVANCED_FACE ( 'NONE', ( #12539 ), #3404, .F. ) ;
#1923 = ORIENTED_EDGE ( 'NONE', *, *, #3172, .F. ) ;
#1924 = CARTESIAN_POINT ( 'NONE',  ( -248.8393377456389146, -10.13317597119169911, 5.948217566906608411 ) ) ;
#1925 = ORIENTED_EDGE ( 'NONE', *, *, #9202, .F. ) ;
#1926 = CARTESIAN_POINT ( 'NONE',  ( 159.4136521835074802, 20.55460285095908191, 207.7919029867859422 ) ) ;
#1927 = CARTESIAN_POINT ( 'NONE',  ( -246.3306884220363315, 9.347001913570167630, -7.525531261512992565 ) ) ;
#1928 = CARTESIAN_POINT ( 'NONE',  ( -197.8197553893924976, 30.00000000000000000, -57.77553482998720114 ) ) ;
#1929 = AXIS2_PLACEMENT_3D ( 'NONE', #5537, #8739, #3733 ) ;
#1930 = DIRECTION ( 'NONE',  ( 1.000000000000000000, 0.000000000000000000, 0.000000000000000000 ) ) ;
#1931 = CARTESIAN_POINT ( 'NONE',  ( -247.5810890934098722, 9.727605306738871249, 7.026623145748954080 ) ) ;
#1932 = AXIS2_PLACEMENT_3D ( 'NONE', #5733, #1606, #2592 ) ;
#1933 = EDGE_CURVE ( 'NONE', #8227, #2601, #7478, .T. ) ;
#1934 = DIRECTION ( 'NONE',  ( 1.047444401652940007E-14, 0.000000000000000000, -1.000000000000000000 ) ) ;
#1935 = CARTESIAN_POINT ( 'NONE',  ( 160.3845033201972115, 9.830508068689120194, 194.1567379014519190 ) ) ;
#1936 = CARTESIAN_POINT ( 'NONE',  ( -229.9928432556552025, -11.86223413274156613, -1.851200411155011771 ) ) ;
#1937 = VERTEX_POINT ( 'NONE', #2658 ) ;
#1938 = ORIENTED_EDGE ( 'NONE', *, *, #7739, .T. ) ;
#1939 = DIRECTION ( 'NONE',  ( -0.000000000000000000, -1.000000000000000000, 0.000000000000000000 ) ) ;
#1940 = DIRECTION ( 'NONE',  ( 0.000000000000000000, 1.000000000000000000, 0.000000000000000000 ) ) ;
#1941 = DIRECTION ( 'NONE',  ( 0.6368676505102716101, 0.000000000000000000, 0.7709731485165527420 ) ) ;
#1942 = CARTESIAN_POINT ( 'NONE',  ( 239.1158061866276228, -0.8260238041387650831, -3.401362076983990512 ) ) ;
#1943 = CARTESIAN_POINT ( 'NONE',  ( 84.02568524182660781, 20.79694577630801078, -247.4557548099990072 ) ) ;
#1944 = VECTOR ( 'NONE', #7171, 1000.000000000000000 ) ;
#1945 = CARTESIAN_POINT ( 'NONE',  ( 71.82423009839129691, 28.60000000000000142, -192.2354503650404922 ) ) ;
#1946 = DIRECTION ( 'NONE',  ( -0.4999999999999919509, 0.000000000000000000, -0.8660254037844432595 ) ) ;
#1947 = CARTESIAN_POINT ( 'NONE',  ( -240.2520669369934865, -3.209691514237213106, 11.31204477728637769 ) ) ;
#1948 = AXIS2_PLACEMENT_3D ( 'NONE', #6107, #6843, #5979 ) ;
#1949 = VERTEX_POINT ( 'NONE', #8510 ) ;
#1950 = ORIENTED_EDGE ( 'NONE', *, *, #1483, .F. ) ;
#1951 = CARTESIAN_POINT ( 'NONE',  ( 220.9845196385168435, -18.00000000000000000, -190.9766794143566528 ) ) ;
#1952 = CARTESIAN_POINT ( 'NONE',  ( -239.1349169607758540, -1.405155705096720498, 11.91743587386434733 ) ) ;
#1953 = VERTEX_POINT ( 'NONE', #12799 ) ;
#1954 = VERTEX_POINT ( 'NONE', #675 ) ;
#1955 = CARTESIAN_POINT ( 'NONE',  ( 193.6077657551222444, -30.00000000000000000, 234.3758371490322929 ) ) ;
#1956 = CARTESIAN_POINT ( 'NONE',  ( 229.9733680233431130, 4.286263893147487610E-16, -3.499999999999964917 ) ) ;
#1957 = CARTESIAN_POINT ( 'NONE',  ( -249.6681481789079555, 11.15796663570597147, 3.682817569140960146 ) ) ;
#1958 =( REPRESENTATION_RELATIONSHIP ('NONE','NONE', #12019, #5191 ) REPRESENTATION_RELATIONSHIP_WITH_TRANSFORMATION ( #5858 )SHAPE_REPRESENTATION_RELATIONSHIP( ) );
#1959 = AXIS2_PLACEMENT_3D ( 'NONE', #4036, #2171, #8184 ) ;
#1960 = CARTESIAN_POINT ( 'NONE',  ( -207.6469600131875666, 19.96883746078517774, 159.3024069659174984 ) ) ;
#1961 = CARTESIAN_POINT ( 'NONE',  ( 0.000000000000000000, 11.79660968244693997, 0.000000000000000000 ) ) ;
#1962 = CARTESIAN_POINT ( 'NONE',  ( -244.0507507057267844, 8.147415050171824547, 8.468315434219642057 ) ) ;
#1963 = ADVANCED_FACE ( 'NONE', ( #6749 ), #4471, .F. ) ;
#1964 = ADVANCED_FACE ( 'NONE', ( #482 ), #12776, .F. ) ;
#1965 = VERTEX_POINT ( 'NONE', #9594 ) ;
#1966 = CARTESIAN_POINT ( 'NONE',  ( -122.2593324768321992, 30.00000000000000000, 168.2755348299905052 ) ) ;
#1967 = CIRCLE ( 'NONE', #12190, 6.500000000000000888 ) ;
#1968 = ORIENTED_EDGE ( 'NONE', *, *, #11546, .F. ) ;
#1969 = CARTESIAN_POINT ( 'NONE',  ( -245.3661487636251479, 8.922833484245296987, -7.644980496657460378 ) ) ;
#1970 = VERTEX_POINT ( 'NONE', #8614 ) ;
#1971 = AXIS2_PLACEMENT_3D ( 'NONE', #12742, #8623, #492 ) ;
#1972 = AXIS2_PLACEMENT_3D ( 'NONE', #12144, #3126, #4939 ) ;
#1973 = EDGE_CURVE ( 'NONE', #2919, #1170, #11616, .T. ) ;
#1974 = CARTESIAN_POINT ( 'NONE',  ( 226.1499999999999773, -1.749660080537334572, 0.03449061573949096376 ) ) ;
#1975 = DIRECTION ( 'NONE',  ( 0.000000000000000000, 0.000000000000000000, 1.000000000000000000 ) ) ;
#1976 = CARTESIAN_POINT ( 'NONE',  ( 239.7985776503625175, 1.848645179571945185, 2.971954070985139751 ) ) ;
#1977 = CARTESIAN_POINT ( 'NONE',  ( -159.3442861576697283, -21.50000000000000000, -192.8974817588416499 ) ) ;
#1978 = CARTESIAN_POINT ( 'NONE',  ( -197.8197553893909912, 29.00000000000000000, 58.77553482999130807 ) ) ;
#1979 = PRODUCT_DEFINITION_SHAPE ( 'NONE', 'NONE',  #13106 ) ;
#1980 = CARTESIAN_POINT ( 'NONE',  ( -239.4323407760790019, 1.761903430914204760, -11.86994927865681149 ) ) ;
#1981 = ORIENTED_EDGE ( 'NONE', *, *, #5179, .F. ) ;
#1982 = CIRCLE ( 'NONE', #7938, 5.099999999999993427 ) ;
#1983 = DIRECTION ( 'NONE',  ( -0.000000000000000000, 0.8560027256360644987, -0.5169713083949903920 ) ) ;
#1984 = EDGE_LOOP ( 'NONE', ( #4294, #12312 ) ) ;
#1985 = CARTESIAN_POINT ( 'NONE',  ( -246.0976122657799010, -9.256780777540988936, -7.636466318229263806 ) ) ;
#1986 = CARTESIAN_POINT ( 'NONE',  ( -249.2714863791443065, -10.50505558484817925, 5.263680432588698110 ) ) ;
#1987 = ORIENTED_EDGE ( 'NONE', *, *, #10581, .F. ) ;
#1988 = EDGE_CURVE ( 'NONE', #10564, #320, #5546, .T. ) ;
#1989 = CIRCLE ( 'NONE', #7312, 6.500000000000005329 ) ;
#1990 = VECTOR ( 'NONE', #3630, 1000.000000000000000 ) ;
#1991 = CARTESIAN_POINT ( 'NONE',  ( 67.61424743001118998, 20.79694577617620155, -252.4341100437179648 ) ) ;
#1992 = EDGE_CURVE ( 'NONE', #7634, #12239, #7667, .T. ) ;
#1993 = CARTESIAN_POINT ( 'NONE',  ( -248.6652334659176802, 9.923450224964128097, -6.747319396128238722 ) ) ;
#1994 = LINE ( 'NONE', #5044, #5513 ) ;
#1995 = VECTOR ( 'NONE', #3341, 1000.000000000000114 ) ;
#1996 = CARTESIAN_POINT ( 'NONE',  ( -244.2512373977512539, -8.280505324001138590, -8.336413190374162951 ) ) ;
#1997 = CARTESIAN_POINT ( 'NONE',  ( -248.5349130529941704, 9.924317173972164952, 6.749248572508020239 ) ) ;
#1998 = DIRECTION ( 'NONE',  ( 0.000000000000000000, 1.000000000000000000, 0.000000000000000000 ) ) ;
#1999 = CARTESIAN_POINT ( 'NONE',  ( 36.24423871767997696, -138.4705547276867321, -20.92562098022514405 ) ) ;
#2000 = CARTESIAN_POINT ( 'NONE',  ( -229.6996680450366171, 1.438960022146944131E-15, 11.75000000000000000 ) ) ;
#2001 = AXIS2_PLACEMENT_3D ( 'NONE', #7473, #2137, #8220 ) ;
#2002 = AXIS2_PLACEMENT_3D ( 'NONE', #4263, #10392, #7336 ) ;
#2003 = CARTESIAN_POINT ( 'NONE',  ( -122.2593324768359935, 30.00000000000000000, -168.2755348299880040 ) ) ;
#2004 = ORIENTED_EDGE ( 'NONE', *, *, #12750, .F. ) ;
#2005 = VERTEX_POINT ( 'NONE', #1741 ) ;
#2006 = CARTESIAN_POINT ( 'NONE',  ( 234.1947771728840166, 20.08915143305504714, -115.4648407707930033 ) ) ;
#2007 = ADVANCED_FACE ( 'NONE', ( #12729 ), #4054, .T. ) ;
#2008 = DIRECTION ( 'NONE',  ( 0.000000000000000000, -0.9998057603070481525, 0.01970892327970899874 ) ) ;
#2009 = CONICAL_SURFACE ( 'NONE', #9393, 250.7000000000000171, 0.7853981633974476129 ) ;
#2010 = DIRECTION ( 'NONE',  ( 0.4503334343941626794, -0.7071067811865380248, 0.5451603414288055394 ) ) ;
#2011 = CARTESIAN_POINT ( 'NONE',  ( 172.3268284089184874, 20.79694577645659948, 196.4640694358555209 ) ) ;
#2012 = EDGE_CURVE ( 'NONE', #3737, #7634, #3665, .T. ) ;
#2013 = DIRECTION ( 'NONE',  ( 0.6368676505102696117, 0.000000000000000000, 0.7709731485165545184 ) ) ;
#2014 = DIRECTION ( 'NONE',  ( 0.9659258262890717539, 0.000000000000000000, -0.2588190451025078609 ) ) ;
#2015 = CARTESIAN_POINT ( 'NONE',  ( -243.6657757798965349, -7.864920284775232417, 8.729522416371102267 ) ) ;
#2016 = CONTEXT_DEPENDENT_SHAPE_REPRESENTATION ( #2263, #4833 ) ;
#2017 = ORIENTED_EDGE ( 'NONE', *, *, #6903, .F. ) ;
#2018 =( REPRESENTATION_RELATIONSHIP ('NONE','NONE', #12019, #182 ) REPRESENTATION_RELATIONSHIP_WITH_TRANSFORMATION ( #8699 )SHAPE_REPRESENTATION_RELATIONSHIP( ) );
#2019 = DIRECTION ( 'NONE',  ( 0.000000000000000000, 0.7071067811865480168, 0.7071067811865470176 ) ) ;
#2020 = CARTESIAN_POINT ( 'NONE',  ( 229.9973251412452839, -3.320720522893729321, 1.129064247440167756 ) ) ;
#2021 = ORIENTED_EDGE ( 'NONE', *, *, #5983, .F. ) ;
#2022 = VERTEX_POINT ( 'NONE', #7736 ) ;
#2023 = DIRECTION ( 'NONE',  ( -0.000000000000000000, -1.000000000000000000, 0.000000000000000000 ) ) ;
#2024 = CARTESIAN_POINT ( 'NONE',  ( -197.8197553893909912, 18.00000000000000000, 64.27553482999130097 ) ) ;
#2025 = CARTESIAN_POINT ( 'NONE',  ( 252.2208631679619941, 20.08915143265656766, 67.55708173926319660 ) ) ;
#2026 = CIRCLE ( 'NONE', #6509, 269.0000000000000000 ) ;
#2027 = DIRECTION ( 'NONE',  ( -0.6368676505102707219, 0.000000000000000000, -0.7709731485165536302 ) ) ;
#2028 = DIRECTION ( 'NONE',  ( 1.000000000000000000, 0.000000000000000000, 0.000000000000000000 ) ) ;
#2029 = CARTESIAN_POINT ( 'NONE',  ( -247.1459274860969231, 9.611803612594441049, 6.758488905887352516 ) ) ;
#2030 = ORIENTED_EDGE ( 'NONE', *, *, #8271, .T. ) ;
#2031 = CARTESIAN_POINT ( 'NONE',  ( 172.0303573358523010, 20.79694577634646180, 196.1676464792607248 ) ) ;
#2032 = ORIENTED_EDGE ( 'NONE', *, *, #11546, .T. ) ;
#2033 = CARTESIAN_POINT ( 'NONE',  ( -246.4294064437368093, 9.379184893845605941, -7.077828147084206378 ) ) ;
#2034 = ORIENTED_EDGE ( 'NONE', *, *, #3107, .T. ) ;
#2035 = CONICAL_SURFACE ( 'NONE', #4796, 5.499999999999998224, 0.7853981633974461696 ) ;
#2036 = EDGE_CURVE ( 'NONE', #6295, #7466, #3961, .T. ) ;
#2037 = DIRECTION ( 'NONE',  ( 0.6368676505102700558, 0.000000000000000000, 0.7709731485165541853 ) ) ;
#2038 = DIRECTION ( 'NONE',  ( 0.6368676505102716101, 0.000000000000000000, 0.7709731485165527420 ) ) ;
#2039 = DIRECTION ( 'NONE',  ( 0.000000000000000000, 0.000000000000000000, 1.000000000000000000 ) ) ;
#2040 = CARTESIAN_POINT ( 'NONE',  ( -122.2593324768321992, 30.00000000000000000, 161.7755348299905052 ) ) ;
#2041 = CARTESIAN_POINT ( 'NONE',  ( -225.7689075324034320, 20.08915143297737060, -130.3442252640567744 ) ) ;
#2042 = DIRECTION ( 'NONE',  ( 0.000000000000000000, 1.000000000000000000, 0.000000000000000000 ) ) ;
#2043 = CARTESIAN_POINT ( 'NONE',  ( -172.0303573358527274, 20.79694577634646535, 196.1676464792603269 ) ) ;
#2044 = ORIENTED_EDGE ( 'NONE', *, *, #657, .T. ) ;
#2045 = CARTESIAN_POINT ( 'NONE',  ( -238.9359159443557701, -1.030912824209149203, -11.70469086939901437 ) ) ;
#2046 = ORIENTED_EDGE ( 'NONE', *, *, #6198, .T. ) ;
#2047 = CARTESIAN_POINT ( 'NONE',  ( -249.7854625207512527, 11.61528754085123616, -1.774251673167930754 ) ) ;
#2048 = DIRECTION ( 'NONE',  ( 8.659560562354913137E-17, -0.7071067811865489050, 0.7071067811865460184 ) ) ;
#2049 = CARTESIAN_POINT ( 'NONE',  ( -249.4806725023741478, -10.78221059150020622, 4.672140297554956412 ) ) ;
#2050 = ORIENTED_EDGE ( 'NONE', *, *, #9486, .F. ) ;
#2051 = EDGE_CURVE ( 'NONE', #3412, #3020, #8534, .T. ) ;
#2052 = CARTESIAN_POINT ( 'NONE',  ( -115.5625104413703923, 20.79694577664888300, 234.3927740973005029 ) ) ;
#2053 = CARTESIAN_POINT ( 'NONE',  ( -246.0505219334675076, 9.238338704539428292, -7.658960896126895790 ) ) ;
#2054 = DIRECTION ( 'NONE',  ( 0.000000000000000000, 0.9998057603070481525, -0.01970892327970899874 ) ) ;
#2055 = CARTESIAN_POINT ( 'NONE',  ( -245.6111173992502756, -9.040876194414714462, -7.505250416031252314 ) ) ;
#2056 = CARTESIAN_POINT ( 'NONE',  ( -247.8923716106052950, 9.795774998289056512, 6.931293060548126661 ) ) ;
#2057 = DIRECTION ( 'NONE',  ( 0.000000000000000000, 0.000000000000000000, -1.000000000000000000 ) ) ;
#2058 = DIRECTION ( 'NONE',  ( 0.8199460427888384251, 0.5538822189107470706, 0.1445786100688183917 ) ) ;
#2059 = EDGE_CURVE ( 'NONE', #4889, #13031, #7123, .T. ) ;
#2060 = DIRECTION ( 'NONE',  ( -0.000000000000000000, 1.000000000000000000, 0.000000000000000000 ) ) ;
#2061 = CONTEXT_DEPENDENT_SHAPE_REPRESENTATION ( #10383, #1870 ) ;
#2062 = ADVANCED_FACE ( 'NONE', ( #6117 ), #2182, .F. ) ;
#2063 = CARTESIAN_POINT ( 'NONE',  ( 153.9282213272189495, -19.40000000000000213, 245.7765299597151341 ) ) ;
#2064 = ORIENTED_EDGE ( 'NONE', *, *, #5815, .F. ) ;
#2065 = ORIENTED_EDGE ( 'NONE', *, *, #8041, .F. ) ;
#2066 = CARTESIAN_POINT ( 'NONE',  ( 196.2980642835735239, 20.08915143291160632, -172.1812796681614941 ) ) ;
#2067 = DIRECTION ( 'NONE',  ( 0.000000000000000000, 0.000000000000000000, 1.000000000000000000 ) ) ;
#2068 = LINE ( 'NONE', #3259, #10208 ) ;
#2069 = CARTESIAN_POINT ( 'NONE',  ( 260.7745447061710138, 20.79694577634646180, 17.06760680878259961 ) ) ;
#2070 = DIRECTION ( 'NONE',  ( 0.000000000000000000, 1.000000000000000000, 0.000000000000000000 ) ) ;
#2071 = CARTESIAN_POINT ( 'NONE',  ( 0.000000000000000000, 0.000000000000000000, 0.000000000000000000 ) ) ;
#2072 = CARTESIAN_POINT ( 'NONE',  ( -244.0876577941736230, -8.170278132102669844, 8.444514123292313101 ) ) ;
#2073 = ITEM_DEFINED_TRANSFORMATION ( 'NONE', 'NONE', #9965,  #805 ) ;
#2074 = EDGE_CURVE ( 'NONE', #5784, #10046, #8107, .T. ) ;
#2075 =( REPRESENTATION_RELATIONSHIP ('NONE','NONE', #12019, #182 ) REPRESENTATION_RELATIONSHIP_WITH_TRANSFORMATION ( #447 )SHAPE_REPRESENTATION_RELATIONSHIP( ) );
#2076 = VERTEX_POINT ( 'NONE', #2568 ) ;
#2077 = PLANE ( 'NONE',  #8082 ) ;
#2078 = LINE ( 'NONE', #1542, #5506 ) ;
#2079 = VERTEX_POINT ( 'NONE', #518 ) ;
#2080 = EDGE_LOOP ( 'NONE', ( #11000, #8423, #6628, #1826 ) ) ;
#2081 = EDGE_CURVE ( 'NONE', #1218, #11098, #384, .T. ) ;
#2082 = DIRECTION ( 'NONE',  ( 0.000000000000000000, 0.9998057603070480415, -0.01970892327970899874 ) ) ;
#2083 = CARTESIAN_POINT ( 'NONE',  ( -197.8197553893909912, 30.00000000000000000, 70.77553482999131518 ) ) ;
#2084 = PRODUCT_DEFINITION_SHAPE ( 'NONE', 'NONE',  #13107 ) ;
#2085 = CARTESIAN_POINT ( 'NONE',  ( -130.8783844626380812, 19.96883746054828279, -226.6392846538615231 ) ) ;
#2086 = CARTESIAN_POINT ( 'NONE',  ( -239.6349225386288708, -1.943794465495108703, -11.84155609468290571 ) ) ;
#2087 = CARTESIAN_POINT ( 'NONE',  ( -245.8608051595201403, 9.153297356747751579, 7.368056653819033741 ) ) ;
#2088 = ORIENTED_EDGE ( 'NONE', *, *, #5129, .T. ) ;
#2089 = CONICAL_SURFACE ( 'NONE', #9340, 249.2999999999999829, 0.7853981633974207455 ) ;
#2090 = DIRECTION ( 'NONE',  ( 0.000000000000000000, 1.000000000000000000, 0.000000000000000000 ) ) ;
#2091 = CIRCLE ( 'NONE', #9537, 231.0000000000000000 ) ;
#2092 = VECTOR ( 'NONE', #5127, 1000.000000000000227 ) ;
#2094 = VERTEX_POINT ( 'NONE', #4310 ) ;
#2093 = AXIS2_PLACEMENT_3D ( 'NONE', #11548, #2402, #9473 ) ;
#2095 = CARTESIAN_POINT ( 'NONE',  ( -0.000000000000000000, -30.00000000000000000, 0.000000000000000000 ) ) ;
#2096 = ORIENTED_EDGE ( 'NONE', *, *, #1439, .T. ) ;
#2097 = DIRECTION ( 'NONE',  ( 0.000000000000000000, 0.9998057603070481525, -0.01970892327970900221 ) ) ;
#2098 =( NAMED_UNIT ( * ) SI_UNIT ( $, .STERADIAN. ) SOLID_ANGLE_UNIT ( ) );
#2099 = CARTESIAN_POINT ( 'NONE',  ( -289.8128292627096130, -30.00000000000000000, 10.41748504886635907 ) ) ;
#2100 = LINE ( 'NONE', #50, #5575 ) ;
#2101 = DIRECTION ( 'NONE',  ( 0.000000000000000000, 1.000000000000000000, 0.000000000000000000 ) ) ;
#2102 = DIRECTION ( 'NONE',  ( 0.000000000000000000, 0.000000000000000000, 1.000000000000000000 ) ) ;
#2103 = AXIS2_PLACEMENT_3D ( 'NONE', #960, #11152, #10021 ) ;
#2104 = CARTESIAN_POINT ( 'NONE',  ( 153.9282213272189495, -30.00000000000000000, 245.7765299597151341 ) ) ;
#2105 = CONTEXT_DEPENDENT_SHAPE_REPRESENTATION ( #7109, #730 ) ;
#2106 = ORIENTED_EDGE ( 'NONE', *, *, #4196, .F. ) ;
#2107 = FACE_OUTER_BOUND ( 'NONE', #1347, .T. ) ;
#2108 = CONICAL_SURFACE ( 'NONE', #3375, 5.100000000000017408, 0.7853981633974503884 ) ;
#2109 = EDGE_CURVE ( 'NONE', #12702, #3706, #11300, .T. ) ;
#2110 = ORIENTED_EDGE ( 'NONE', *, *, #10806, .T. ) ;
#2111 = CARTESIAN_POINT ( 'NONE',  ( -210.0000000000000000, 28.60000000000000142, 0.000000000000000000 ) ) ;
#2112 = CARTESIAN_POINT ( 'NONE',  ( -243.0176490148521395, -7.336472068459895191, -9.496559186012056841 ) ) ;
#2113 = AXIS2_PLACEMENT_3D ( 'NONE', #1306, #6378, #9442 ) ;
#2114 = CARTESIAN_POINT ( 'NONE',  ( -248.3532242370870620, -9.880481159896127963, 6.359788946042714386 ) ) ;
#2115 = ORIENTED_EDGE ( 'NONE', *, *, #11514, .T. ) ;
#2116 = CARTESIAN_POINT ( 'NONE',  ( 247.4557548102664839, 20.79694577621951979, -84.02568524171830688 ) ) ;
#2117 = CARTESIAN_POINT ( 'NONE',  ( -245.5461639313797377, 9.015782184433717816, -7.919169856962964715 ) ) ;
#2118 = CARTESIAN_POINT ( 'NONE',  ( 235.4000000000000057, -0.1024105694488001289, -5.195143123655522110 ) ) ;
#2119 = CARTESIAN_POINT ( 'NONE',  ( -242.9798744230415934, -7.293926269598956402, -9.214525213004751691 ) ) ;
#2120 = CIRCLE ( 'NONE', #2549, 5.500000000000015099 ) ;
#2121 = DIRECTION ( 'NONE',  ( 0.6368676505102706109, 0.000000000000000000, 0.7709731485165535192 ) ) ;
#2122 = CARTESIAN_POINT ( 'NONE',  ( 41.69198534955599911, -138.4705547276867321, 3.647576077975493547 ) ) ;
#2123 = ADVANCED_FACE ( 'NONE', ( #8519 ), #2981, .T. ) ;
#2124 = DIRECTION ( 'NONE',  ( -0.000000000000000000, -1.000000000000000000, 0.000000000000000000 ) ) ;
#2125 = EDGE_CURVE ( 'NONE', #3954, #3345, #11078, .T. ) ;
#2126 = CIRCLE ( 'NONE', #5099, 245.7999999999999829 ) ;
#2127 = ITEM_DEFINED_TRANSFORMATION ( 'NONE', 'NONE', #2975,  #805 ) ;
#2128 = B_SPLINE_CURVE_WITH_KNOTS ( 'NONE', 3,
 ( #7950, #1947, #7151, #8153, #7215, #5067, #12148, #11146, #4066, #10272, #5007, #4003, #6217, #9144, #4075, #3129, #1147, #11281, #3943, #10013, #1078, #8084, #6021, #5136, #9212, #8965, #89, #4143, #20, #12219, #3070, #2015, #12021, #10079, #11208, #2072, #2141, #6150, #2999, #6087, #7082, #10204, #8224, #5953, #2867, #951, #6952, #8952, #13013, #3877, #11008, #1881, #882, #4943, #4272, #1411, #5472, #5273, #10541, #9530, #6416, #9347, #152, #2212, #3394, #7347, #12476 ),
 .UNSPECIFIED., .F., .F.,
 ( 4, 2, 2, 1, 1, 1, 1, 2, 2, 2, 2, 2, 1, 1, 1, 1, 1, 2, 2, 2, 2, 2, 1, 1, 1, 2, 2, 2, 2, 1, 1, 1, 1, 2, 2, 2, 2, 1, 1, 1, 2, 2, 4 ),
 ( 0.000000000000000000, 0.1249999999996426747, 0.1874999999994641231, 0.2187499999993749999, 0.2343749999993287592, 0.2421874999993055833, 0.2460937499992956190, 0.2480468749992907895, 0.2499999999992859601, 0.3749999999989899191, 0.4374999999988398169, 0.4687499999987648214, 0.4843749999987274069, 0.4921874999987085886, 0.4960937499986973198, 0.4980468749986917687, 0.4990234374986870503, 0.4995117187486847743, 0.4999999999986824983, 0.5624999999989823696, 0.5937499999991320276, 0.6093749999992053024, 0.6171874999992403854, 0.6210937499992564836, 0.6230468749992645883, 0.6240234374992686961, 0.6249999999992726929, 0.6874999999994171329, 0.7187499999994895195, 0.7343749999995224931, 0.7421874999995388134, 0.7460937499995505817, 0.7480468749995564659, 0.7490234374995594635, 0.7499999999995624611, 0.8124999999996862510, 0.8437499999997453148, 0.8593749999997780664, 0.8671874999997977174, 0.8710937499998041567, 0.8730468749998074873, 0.8749999999998107070, 1.000000000000000000 ),
 .UNSPECIFIED. ) ;
#2129 = DIRECTION ( 'NONE',  ( 0.000000000000000000, 0.000000000000000000, 1.000000000000000000 ) ) ;
#2130 = ORIENTED_EDGE ( 'NONE', *, *, #8273, .F. ) ;
#2131 = VERTEX_POINT ( 'NONE', #6454 ) ;
#2132 = CARTESIAN_POINT ( 'NONE',  ( -258.8746690723625079, 20.08915143294039396, -34.10614053585524630 ) ) ;
#2133 = DIRECTION ( 'NONE',  ( 0.000000000000000000, 0.000000000000000000, 1.000000000000000000 ) ) ;
#2134 = EDGE_CURVE ( 'NONE', #11817, #3319, #10441, .T. ) ;
#2135 = CARTESIAN_POINT ( 'NONE',  ( 239.1818646735635241, -0.9924701939322742028, -3.356351167340032138 ) ) ;
#2136 = AXIS2_PLACEMENT_3D ( 'NONE', #9865, #10000, #9792 ) ;
#2137 = DIRECTION ( 'NONE',  ( -1.000000000000000000, 0.000000000000000000, 0.000000000000000000 ) ) ;
#2138 = CARTESIAN_POINT ( 'NONE',  ( 226.3083638770190191, 20.79694577655596888, 130.6873781509345918 ) ) ;
#2139 = CARTESIAN_POINT ( 'NONE',  ( -210.0000000000000000, 28.60000000000000142, -5.100000000000000533 ) ) ;
#2140 = DIRECTION ( 'NONE',  ( 0.7071067811865389130, 0.000000000000000000, 0.7071067811865561215 ) ) ;
#2141 = CARTESIAN_POINT ( 'NONE',  ( -244.1571280462642619, -8.217568831514851624, 8.398466974160381682 ) ) ;
#2142 = EDGE_LOOP ( 'NONE', ( #6103, #9301, #10192, #11179 ) ) ;
#2143 = DIRECTION ( 'NONE',  ( 0.000000000000000000, 1.000000000000000000, 0.000000000000000000 ) ) ;
#2144 = CARTESIAN_POINT ( 'NONE',  ( -239.1938262336951482, 1.469859129952955312, 11.65770207320726470 ) ) ;
#2145 = CARTESIAN_POINT ( 'NONE',  ( 229.9750439289697113, -0.9060155281103843272, 3.388384136948113579 ) ) ;
#2146 = ORIENTED_EDGE ( 'NONE', *, *, #2336, .T. ) ;
#2147 = ORIENTED_EDGE ( 'NONE', *, *, #7598, .T. ) ;
#2148 = CARTESIAN_POINT ( 'NONE',  ( 222.0845275804282153, 1.749660080537334128, -0.03449061573949074866 ) ) ;
#2149 = CARTESIAN_POINT ( 'NONE',  ( -249.7999999999999829, 22.00000000000000000, 0.000000000000000000 ) ) ;
#2150 = ADVANCED_FACE ( 'NONE', ( #10709 ), #10446, .F. ) ;
#2151 = EDGE_CURVE ( 'NONE', #8455, #10757, #639, .T. ) ;
#2152 = CARTESIAN_POINT ( 'NONE',  ( -172.5787240286020392, 19.96883746144090210, 196.7513681798772609 ) ) ;
#2153 =( REPRESENTATION_RELATIONSHIP ('NONE','NONE', #12019, #5191 ) REPRESENTATION_RELATIONSHIP_WITH_TRANSFORMATION ( #5736 )SHAPE_REPRESENTATION_RELATIONSHIP( ) );
#2154 = AXIS2_PLACEMENT_3D ( 'NONE', #9103, #9171, #4969 ) ;
#2155 = ORIENTED_EDGE ( 'NONE', *, *, #8928, .T. ) ;
#2156 = CARTESIAN_POINT ( 'NONE',  ( -239.4338636940265133, -1.763423114931361946, -11.86972337156385393 ) ) ;
#2157 = DIRECTION ( 'NONE',  ( 0.8191520442889910214, 0.000000000000000000, 0.5735764363510471586 ) ) ;
#2158 = CARTESIAN_POINT ( 'NONE',  ( -241.8928034524436441, 6.135811581234290379, 10.02290695385687158 ) ) ;
#2159 = ORIENTED_EDGE ( 'NONE', *, *, #6882, .F. ) ;
#2160 = CARTESIAN_POINT ( 'NONE',  ( 107.6783259591029065, 20.79694577634646535, 237.6585102388686153 ) ) ;
#2162 = ORIENTED_EDGE ( 'NONE', *, *, #6885, .F. ) ;
#2161 = AXIS2_PLACEMENT_3D ( 'NONE', #3025, #3094, #7305 ) ;
#2163 = LINE ( 'NONE', #11502, #8842 ) ;
#2164 = ORIENTED_EDGE ( 'NONE', *, *, #5806, .F. ) ;
#2165 = VERTEX_POINT ( 'NONE', #2505 ) ;
#2166 = AXIS2_PLACEMENT_3D ( 'NONE', #10042, #6049, #3228 ) ;
#2167 = CARTESIAN_POINT ( 'NONE',  ( 229.9000000000000057, 4.550331206106116078, 2.508881407069060376 ) ) ;
#2168 = EDGE_CURVE ( 'NONE', #11817, #6957, #8586, .T. ) ;
#2169 = FILL_AREA_STYLE ('',( #114 ) ) ;
#2170 = CARTESIAN_POINT ( 'NONE',  ( 239.1158061866188405, 0.8260238041136663822, 3.401362076984711269 ) ) ;
#2171 = DIRECTION ( 'NONE',  ( 1.000000000000000000, 0.000000000000000000, 0.000000000000000000 ) ) ;
#2172 = CARTESIAN_POINT ( 'NONE',  ( -151.8458048843641848, 20.08915143297736705, -211.9058003148608407 ) ) ;
#2173 = LINE ( 'NONE', #7116, #7927 ) ;
#2174 = AXIS2_PLACEMENT_3D ( 'NONE', #12269, #4260, #3186 ) ;
#2175 = ITEM_DEFINED_TRANSFORMATION ( 'NONE', 'NONE', #2706,  #805 ) ;
#2176 = ORIENTED_EDGE ( 'NONE', *, *, #9731, .T. ) ;
#2177 = DIRECTION ( 'NONE',  ( 0.000000000000000000, 1.000000000000000000, 0.000000000000000000 ) ) ;
#2178 = CIRCLE ( 'NONE', #700, 6.500000000000000000 ) ;
#2179 = ORIENTED_EDGE ( 'NONE', *, *, #1023, .F. ) ;
#2180 = CIRCLE ( 'NONE', #3024, 239.8169934640465044 ) ;
#2181 = LINE ( 'NONE', #1383, #11686 ) ;
#2182 = CYLINDRICAL_SURFACE ( 'NONE', #12147, 5.499999999999998224 ) ;
#2183 = CARTESIAN_POINT ( 'NONE',  ( -248.0831933713610056, -9.830508068705269054, 6.436117704883859147 ) ) ;
#2184 = VERTEX_POINT ( 'NONE', #2442 ) ;
#2185 = CARTESIAN_POINT ( 'NONE',  ( -234.3927740973375080, 20.79694577663154575, -115.5625104413860100 ) ) ;
#2186 = CARTESIAN_POINT ( 'NONE',  ( -244.2463344858503831, 8.285434993257245750, -8.680536399821541238 ) ) ;
#2187 = LINE ( 'NONE', #10579, #4236 ) ;
#2188 =( REPRESENTATION_RELATIONSHIP ('NONE','NONE', #12019, #5191 ) REPRESENTATION_RELATIONSHIP_WITH_TRANSFORMATION ( #5606 )SHAPE_REPRESENTATION_RELATIONSHIP( ) );
#2189 = CARTESIAN_POINT ( 'NONE',  ( -246.7009519929982275, -9.473788075376265994, -6.950529151851262633 ) ) ;
#2190 = COLOUR_RGB ( '', 0.31764706, 0.68627451, 0.89019608) ;
#2191 = CARTESIAN_POINT ( 'NONE',  ( 239.1299809605872326, -0.8683754750072776307, 3.391597751362151580 ) ) ;
#2192 = DIRECTION ( 'NONE',  ( 0.5887335932212847123, 0.5538822189107470706, 0.5887335932212990341 ) ) ;
#2193 = CARTESIAN_POINT ( 'NONE',  ( 240.5112511684932883, 3.170498835030340690, 1.486196988727406465 ) ) ;
#2194 = ITEM_DEFINED_TRANSFORMATION ( 'NONE', 'NONE', #16,  #805 ) ;
#2195 = CIRCLE ( 'NONE', #9866, 1.750000000000000000 ) ;
#2196 = CIRCLE ( 'NONE', #7959, 6.500000000000005329 ) ;
#2197 = DIRECTION ( 'NONE',  ( 0.000000000000000000, -1.000000000000000000, 0.000000000000000000 ) ) ;
#2198 = CIRCLE ( 'NONE', #10078, 250.3823410207189966 ) ;
#2199 = EDGE_LOOP ( 'NONE', ( #2226, #4900, #6796, #3552 ) ) ;
#2200 = CARTESIAN_POINT ( 'NONE',  ( 34.10614053541959834, 20.08915143339292442, 258.8746690701424882 ) ) ;
#2201 = LINE ( 'NONE', #12405, #6580 ) ;
#2202 = AXIS2_PLACEMENT_3D ( 'NONE', #1816, #1675, #613 ) ;
#2203 = EDGE_CURVE ( 'NONE', #10757, #12935, #1318, .T. ) ;
#2204 = LINE ( 'NONE', #4264, #3582 ) ;
#2205 = EDGE_CURVE ( 'NONE', #9116, #7165, #10575, .T. ) ;
#2206 = CARTESIAN_POINT ( 'NONE',  ( 239.4370728335728700, -1.442813601772337639, -3.188799201155995355 ) ) ;
#2207 = CARTESIAN_POINT ( 'NONE',  ( 71.82423009839129691, 19.40000000000000213, 202.4354503650404808 ) ) ;
#2208 = CARTESIAN_POINT ( 'NONE',  ( -248.1924789821139825, -9.852676062999542239, 6.850256174357434169 ) ) ;
#2209 = CIRCLE ( 'NONE', #4129, 5.500000000000005329 ) ;
#2210 = CARTESIAN_POINT ( 'NONE',  ( 136.1890905123932498, -22.00000000000000000, -208.4551069784743333 ) ) ;
#2211 = DIRECTION ( 'NONE',  ( 0.9961946980917466554, 0.000000000000000000, -0.08715574274764503748 ) ) ;
#2212 = CARTESIAN_POINT ( 'NONE',  ( -246.6693634554316645, -9.463199073330141431, 6.964939579038730955 ) ) ;
#2213 = ORIENTED_EDGE ( 'NONE', *, *, #1419, .F. ) ;
#2214 = CARTESIAN_POINT ( 'NONE',  ( 71.82423009839129691, 18.00000000000000000, 197.3354503650404865 ) ) ;
#2215 = CARTESIAN_POINT ( 'NONE',  ( 229.9884488601945236, -2.638803137220849138, -2.310864750561204772 ) ) ;
#2216 = ORIENTED_EDGE ( 'NONE', *, *, #2809, .T. ) ;
#2217 = ORIENTED_EDGE ( 'NONE', *, *, #12585, .T. ) ;
#2218 = CIRCLE ( 'NONE', #8197, 3.153020646647511249 ) ;
#2219 = DIRECTION ( 'NONE',  ( 0.000000000000000000, 0.000000000000000000, 1.000000000000000000 ) ) ;
#2220 = DIRECTION ( 'NONE',  ( 0.6368676505102696117, 0.000000000000000000, 0.7709731485165545184 ) ) ;
#2221 = CARTESIAN_POINT ( 'NONE',  ( 252.8031682264634981, 19.96883746174475860, 67.71318189738019555 ) ) ;
#2222 = DIRECTION ( 'NONE',  ( 0.000000000000000000, 1.000000000000000000, 0.000000000000000000 ) ) ;
#2223 = CARTESIAN_POINT ( 'NONE',  ( 0.000000000000000000, 0.000000000000000000, 0.000000000000000000 ) ) ;
#2224 = CARTESIAN_POINT ( 'NONE',  ( -244.4357566151503534, 8.400224619627458367, 8.216123740249937413 ) ) ;
#2225 = VECTOR ( 'NONE', #5206, 1000.000000000000114 ) ;
#2226 = ORIENTED_EDGE ( 'NONE', *, *, #7100, .F. ) ;
#2227 = CARTESIAN_POINT ( 'NONE',  ( -210.0000000000000000, 18.00000000000000000, -6.500000000000007994 ) ) ;
#2228 = EDGE_CURVE ( 'NONE', #8768, #2870, #12765, .T. ) ;
#2229 = ORIENTED_EDGE ( 'NONE', *, *, #2803, .F. ) ;
#2230 = EDGE_CURVE ( 'NONE', #6421, #10706, #10641, .T. ) ;
#2231 = DIRECTION ( 'NONE',  ( 0.000000000000000000, 1.000000000000000000, 0.000000000000000000 ) ) ;
#2232 = EDGE_LOOP ( 'NONE', ( #7992, #8033 ) ) ;
#2233 = VERTEX_POINT ( 'NONE', #8458 ) ;
#2234 = VECTOR ( 'NONE', #7871, 1000.000000000000000 ) ;
#2235 = DIRECTION ( 'NONE',  ( 0.000000000000000000, 0.000000000000000000, 1.000000000000000000 ) ) ;
#2236 = CARTESIAN_POINT ( 'NONE',  ( 0.000000000000000000, 0.000000000000000000, 0.000000000000000000 ) ) ;
#2237 = PRODUCT_DEFINITION_SHAPE ( 'NONE', 'NONE',  #13069 ) ;
#2238 = CARTESIAN_POINT ( 'NONE',  ( -286.5648042451072115, -30.00000000000000000, 14.34944810630078393 ) ) ;
#2239 = CARTESIAN_POINT ( 'NONE',  ( 239.4793126112416246, 1.500292816075383895, -3.162144597818810077 ) ) ;
#2240 = CARTESIAN_POINT ( 'NONE',  ( -24.18668477630637526, -19.00000000000000000, 294.9245348571438967 ) ) ;
#2241 = DIRECTION ( 'NONE',  ( 0.6368676505102708330, 0.000000000000000000, 0.7709731485165535192 ) ) ;
#2242 = CONTEXT_DEPENDENT_SHAPE_REPRESENTATION ( #10081, #3397 ) ;
#2243 = ORIENTED_EDGE ( 'NONE', *, *, #4967, .F. ) ;
#2244 = DIRECTION ( 'NONE',  ( 0.000000000000000000, 0.01970892327970899874, 0.9998057603070481525 ) ) ;
#2245 = EDGE_LOOP ( 'NONE', ( #10390, #7652, #3647, #709 ) ) ;
#2246 = ADVANCED_FACE ( 'NONE', ( #1446 ), #3391, .F. ) ;
#2247 = AXIS2_PLACEMENT_3D ( 'NONE', #8902, #7107, #4825 ) ;
#2248 = DIRECTION ( 'NONE',  ( 0.000000000000000000, 1.000000000000000000, 0.000000000000000000 ) ) ;
#2249 = CARTESIAN_POINT ( 'NONE',  ( -244.7604950959731696, -8.603785961650375569, -8.365103762956266564 ) ) ;
#2250 = CARTESIAN_POINT ( 'NONE',  ( 221.3800702329289720, 20.08915143297736705, -137.6665579279351732 ) ) ;
#2251 = ORIENTED_EDGE ( 'NONE', *, *, #1303, .T. ) ;
#2252 = EDGE_CURVE ( 'NONE', #5570, #1246, #8724, .T. ) ;
#2253 = CARTESIAN_POINT ( 'NONE',  ( 196.4640694355999813, 20.79694577639575570, -172.3268284093740021 ) ) ;
#2254 = CARTESIAN_POINT ( 'NONE',  ( -240.5118714936659501, 3.871746541805194841, -11.35824976271609188 ) ) ;
#2255 = DIRECTION ( 'NONE',  ( 0.000000000000000000, 0.000000000000000000, 1.000000000000000000 ) ) ;
#2256 = CARTESIAN_POINT ( 'NONE',  ( -242.2247058965992608, -6.524571383558081195, -9.772025480106055539 ) ) ;
#2257 =( NAMED_UNIT ( * ) SI_UNIT ( $, .STERADIAN. ) SOLID_ANGLE_UNIT ( ) );
#2258 = CARTESIAN_POINT ( 'NONE',  ( -229.7631465151204679, 5.933468005304723292, -10.43713253351459080 ) ) ;
#2259 = DIRECTION ( 'NONE',  ( 0.000000000000000000, 0.000000000000000000, 1.000000000000000000 ) ) ;
#2260 = ORIENTED_EDGE ( 'NONE', *, *, #14, .T. ) ;
#2261 = CARTESIAN_POINT ( 'NONE',  ( 17.05314194221880086, 20.08915143297735284, -260.5542428351129729 ) ) ;
#2262 = CYLINDRICAL_SURFACE ( 'NONE', #10521, 230.0000000000000000 ) ;
#2263 =( REPRESENTATION_RELATIONSHIP ('NONE','NONE', #12019, #182 ) REPRESENTATION_RELATIONSHIP_WITH_TRANSFORMATION ( #10205 )SHAPE_REPRESENTATION_RELATIONSHIP( ) );
#2264 = CARTESIAN_POINT ( 'NONE',  ( -248.7900388717503404, 10.10208648674501219, 6.000868149965899789 ) ) ;
#2265 = DIRECTION ( 'NONE',  ( 0.000000000000000000, -1.000000000000000000, 0.000000000000000000 ) ) ;
#2266 = LINE ( 'NONE', #5202, #5199 ) ;
#2267 = CARTESIAN_POINT ( 'NONE',  ( -247.0023889732649991, -9.573823398995038758, 7.235426325582930751 ) ) ;
#2268 = DIRECTION ( 'NONE',  ( 0.000000000000000000, 1.000000000000000000, 0.000000000000000000 ) ) ;
#2269 = DIRECTION ( 'NONE',  ( 0.8660254037844380415, 0.000000000000000000, 0.5000000000000009992 ) ) ;
#2270 = CARTESIAN_POINT ( 'NONE',  ( 153.9282213272189495, -19.40000000000000213, 245.7765299597151341 ) ) ;
#2271 = EDGE_LOOP ( 'NONE', ( #3914, #9287 ) ) ;
#2272 = FACE_OUTER_BOUND ( 'NONE', #6185, .T. ) ;
#2273 = EDGE_CURVE ( 'NONE', #12270, #12220, #5318, .T. ) ;
#2274 = CARTESIAN_POINT ( 'NONE',  ( 229.9996516955224877, -3.477323162167160753, -0.4589134507980298650 ) ) ;
#2275 = VERTEX_POINT ( 'NONE', #3364 ) ;
#2276 = EDGE_LOOP ( 'NONE', ( #679, #4432, #859, #9482 ) ) ;
#2277 = DIRECTION ( 'NONE',  ( 0.4503334343941562401, 0.7071067811865480168, 0.5451603414287978788 ) ) ;
#2278 = DIRECTION ( 'NONE',  ( 0.000000000000000000, 0.000000000000000000, -1.000000000000000000 ) ) ;
#2279 = PRODUCT_DEFINITION_CONTEXT ( 'detailed design', #6854, 'design' ) ;
#2280 = CARTESIAN_POINT ( 'NONE',  ( -1.009183486025028462E-12, 20.55460285106647689, 261.3381329044966606 ) ) ;
#2281 = AXIS2_PLACEMENT_3D ( 'NONE', #5729, #3855, #12860 ) ;
#2282 = CARTESIAN_POINT ( 'NONE',  ( -0.000000000000000000, -18.00000000000000000, 0.000000000000000000 ) ) ;
#2283 = DIRECTION ( 'NONE',  ( 0.000000000000000000, 0.9998057603070481525, -0.01970892327970900221 ) ) ;
#2284 = ORIENTED_EDGE ( 'NONE', *, *, #11862, .F. ) ;
#2285 = CARTESIAN_POINT ( 'NONE',  ( 0.000000000000000000, 0.000000000000000000, -11.75000000000000000 ) ) ;
#2286 = EDGE_CURVE ( 'NONE', #9966, #4005, #12133, .T. ) ;
#2287 = ORIENTED_EDGE ( 'NONE', *, *, #3305, .T. ) ;
#2288 = DIRECTION ( 'NONE',  ( 0.000000000000000000, 1.000000000000000000, 0.000000000000000000 ) ) ;
#2289 = ORIENTED_EDGE ( 'NONE', *, *, #7425, .T. ) ;
#2290 = EDGE_LOOP ( 'NONE', ( #10173, #6761, #12594, #2808 ) ) ;
#2291 = AXIS2_PLACEMENT_3D ( 'NONE', #11693, #1552, #1486 ) ;
#2292 = CARTESIAN_POINT ( 'NONE',  ( 122.2593324768346008, 30.00000000000000000, 168.2755348299889988 ) ) ;
#2293 = DIRECTION ( 'NONE',  ( 0.000000000000000000, -1.000000000000000000, 0.000000000000000000 ) ) ;
#2294 = ADVANCED_FACE ( 'NONE', ( #11521 ), #5514, .F. ) ;
#2295 = CARTESIAN_POINT ( 'NONE',  ( 239.4650615381723355, 1.481238645322935588, -3.171113114083459639 ) ) ;
#2296 = B_SPLINE_CURVE_WITH_KNOTS ( 'NONE', 3,
 ( #8985, #11943, #10167, #6002, #12117, #3037, #1046, #7120, #7914, #4841, #5037, #6057, #11178, #9985, #4043, #12050, #8920, #1920, #2045, #10984, #1856, #7845, #9917, #11113, #5921, #6985, #5105, #12983, #8119, #2970, #854, #10110 ),
 .UNSPECIFIED., .F., .F.,
 ( 4, 2, 2, 1, 1, 2, 2, 2, 2, 1, 2, 2, 2, 2, 1, 1, 1, 2, 4 ),
 ( 0.000000000000000000, 0.06250953600675514255, 0.09376430401013917393, 0.1093916880118240981, 0.1172053800126664769, 0.1211122260130798878, 0.1250190720134933264, 0.1875286080200248562, 0.2187833760232906488, 0.2344107600249281387, 0.2422244520257468836, 0.2500381440265656563, 0.3750572160396264954, 0.4375667520461548610, 0.4688215200494180168, 0.4844489040510496225, 0.4922625960518653976, 0.4961694420522733129, 0.5000762880526811172 ),
 .UNSPECIFIED. ) ;
#2297 = CARTESIAN_POINT ( 'NONE',  ( -239.0839753095793014, 1.310033608828027774, -11.67696114067532775 ) ) ;
#2298 = CARTESIAN_POINT ( 'NONE',  ( -246.8626574257879156, 9.530421749008032961, 7.291787928144687569 ) ) ;
#2299 = DIRECTION ( 'NONE',  ( 0.6368676505102700558, 0.000000000000000000, 0.7709731485165541853 ) ) ;
#2300 = AXIS2_PLACEMENT_3D ( 'NONE', #12226, #4281, #8361 ) ;
#2301 = AXIS2_PLACEMENT_3D ( 'NONE', #3069, #7279, #151 ) ;
#2302 = ORIENTED_EDGE ( 'NONE', *, *, #3436, .F. ) ;
#2303 = DIRECTION ( 'NONE',  ( 0.000000000000000000, -1.000000000000000000, 0.000000000000000000 ) ) ;
#2304 = EDGE_LOOP ( 'NONE', ( #6718, #6456, #12577, #729 ) ) ;
#2305 = CARTESIAN_POINT ( 'NONE',  ( 0.000000000000000000, -20.69999999999999929, 0.000000000000000000 ) ) ;
#2306 = DIRECTION ( 'NONE',  ( -0.4503334343941691187, -0.7071067811865280328, -0.5451603414288131999 ) ) ;
#2307 = CARTESIAN_POINT ( 'NONE',  ( 91.83222442980247990, 20.08915143297736705, -243.9837273761028769 ) ) ;
#2308 = ORIENTED_EDGE ( 'NONE', *, *, #5737, .F. ) ;
#2309 = AXIS2_PLACEMENT_3D ( 'NONE', #10771, #6521, #12769 ) ;
#2310 = AXIS2_PLACEMENT_3D ( 'NONE', #9323, #12193, #2980 ) ;
#2311 = DIRECTION ( 'NONE',  ( 0.6368676505102700558, 0.000000000000000000, 0.7709731485165541853 ) ) ;
#2312 = CARTESIAN_POINT ( 'NONE',  ( -243.4994605516075978, 7.743136871922250641, -9.167522614886454591 ) ) ;
#2313 = DIRECTION ( 'NONE',  ( 0.000000000000000000, 1.000000000000000000, 0.000000000000000000 ) ) ;
#2314 = CIRCLE ( 'NONE', #11256, 239.8169934640465044 ) ;
#2315 = EDGE_CURVE ( 'NONE', #3553, #5907, #7481, .T. ) ;
#2316 = CARTESIAN_POINT ( 'NONE',  ( 71.82423009839129691, 30.00000000000000000, 197.3354503650404865 ) ) ;
#2317 = VECTOR ( 'NONE', #6829, 1000.000000000000000 ) ;
#2318 = ADVANCED_FACE ( 'NONE', ( #328 ), #7387, .F. ) ;
#2319 = AXIS2_PLACEMENT_3D ( 'NONE', #1799, #8861, #470 ) ;
#2320 = CIRCLE ( 'NONE', #2733, 6.500000000000005329 ) ;
#2321 =( LENGTH_UNIT ( ) NAMED_UNIT ( * ) SI_UNIT ( .MILLI., .METRE. ) );
#2322 = SHAPE_DEFINITION_REPRESENTATION ( #10544, #11596 ) ;
#2323 = CARTESIAN_POINT ( 'NONE',  ( -229.6889200636375108, 1.000000000000000000, -11.95826074310140008 ) ) ;
#2324 = ADVANCED_FACE ( 'NONE', ( #1515 ), #12456, .T. ) ;
#2325 = CONTEXT_DEPENDENT_SHAPE_REPRESENTATION ( #6311, #797 ) ;
#2326 = AXIS2_PLACEMENT_3D ( 'NONE', #649, #3571, #4700 ) ;
#2327 = MECHANICAL_DESIGN_GEOMETRIC_PRESENTATION_REPRESENTATION (  '', ( #32 ), #8930 ) ;
#2328 = DIRECTION ( 'NONE',  ( 0.000000000000000000, 0.000000000000000000, 1.000000000000000000 ) ) ;
#2329 = ORIENTED_EDGE ( 'NONE', *, *, #1758, .T. ) ;
#2330 = CARTESIAN_POINT ( 'NONE',  ( 84.14846197979342435, 19.96883746137058679, -247.8175805188673735 ) ) ;
#2331 = CARTESIAN_POINT ( 'NONE',  ( 190.1049936773181628, -18.00000000000000000, 230.1354848321892632 ) ) ;
#2332 = CARTESIAN_POINT ( 'NONE',  ( 0.000000000000000000, -23.50000000000000000, 0.000000000000000000 ) ) ;
#2333 = APPLICATION_CONTEXT ( 'automotive_design' ) ;
#2334 = CARTESIAN_POINT ( 'NONE',  ( 226.1499999999999773, 0.000000000000000000, 0.000000000000000000 ) ) ;
#2335 = CIRCLE ( 'NONE', #6388, 251.8333333333380608 ) ;
#2336 = EDGE_CURVE ( 'NONE', #3553, #900, #3508, .T. ) ;
#2337 = CARTESIAN_POINT ( 'NONE',  ( -210.0000000000000000, 30.00000000000000000, 0.000000000000000000 ) ) ;
#2338 = VECTOR ( 'NONE', #251, 1000.000000000000000 ) ;
#2339 = CARTESIAN_POINT ( 'NONE',  ( 189.4681260268079086, -29.00000000000000000, 229.3645116836727027 ) ) ;
#2340 = DIRECTION ( 'NONE',  ( 0.08715574274765502949, 0.000000000000000000, 0.9961946980917457672 ) ) ;
#2341 = DIRECTION ( 'NONE',  ( 0.6368676505102689456, 0.000000000000000000, 0.7709731485165549625 ) ) ;
#2342 = EDGE_LOOP ( 'NONE', ( #8244, #9820 ) ) ;
#2343 = CARTESIAN_POINT ( 'NONE',  ( 240.4535390813941831, -3.009067775125233712, 1.828999330899334863 ) ) ;
#2344 = CIRCLE ( 'NONE', #8732, 3.153020646647511249 ) ;
#2345 = PRODUCT_DEFINITION_SHAPE ( 'NONE', 'NONE',  #10447 ) ;
#2346 = CARTESIAN_POINT ( 'NONE',  ( 122.2593324768346008, 30.00000000000000000, 161.7755348299889988 ) ) ;
#2347 = ORIENTED_EDGE ( 'NONE', *, *, #4320, .T. ) ;
#2348 = ORIENTED_EDGE ( 'NONE', *, *, #12233, .F. ) ;
#2349 = AXIS2_PLACEMENT_3D ( 'NONE', #10597, #11475, #2340 ) ;
#2350 = FACE_OUTER_BOUND ( 'NONE', #4082, .T. ) ;
#2351 = FACE_BOUND ( 'NONE', #5773, .T. ) ;
#2352 = AXIS2_PLACEMENT_3D ( 'NONE', #1384, #10514, #9510 ) ;
#2353 = CARTESIAN_POINT ( 'NONE',  ( -207.7919029844864269, 20.55460285060714654, 159.4136521835260112 ) ) ;
#2354 = DIRECTION ( 'NONE',  ( -0.000000000000000000, -1.000000000000000000, 0.000000000000000000 ) ) ;
#2355 = DIRECTION ( 'NONE',  ( -0.7660444431189813441, 0.000000000000000000, 0.6427876096865353661 ) ) ;
#2356 = CARTESIAN_POINT ( 'NONE',  ( 235.4000000000000057, 0.000000000000000000, 0.000000000000000000 ) ) ;
#2357 = CARTESIAN_POINT ( 'NONE',  ( -244.1900186690934902, 20.79694577634646535, -91.90986972409987743 ) ) ;
#2358 = AXIS2_PLACEMENT_3D ( 'NONE', #2071, #12280, #4002 ) ;
#2359 = ORIENTED_EDGE ( 'NONE', *, *, #8441, .F. ) ;
#2360 = CARTESIAN_POINT ( 'NONE',  ( 254.0989678903619051, 20.79694577634646890, -59.24444182677473947 ) ) ;
#2361 = VERTEX_POINT ( 'NONE', #454 ) ;
#2362 = CARTESIAN_POINT ( 'NONE',  ( 222.0845275804282153, 0.000000000000000000, 0.000000000000000000 ) ) ;
#2363 = ORIENTED_EDGE ( 'NONE', *, *, #5955, .T. ) ;
#2364 = ORIENTED_EDGE ( 'NONE', *, *, #10139, .F. ) ;
#2365 = CARTESIAN_POINT ( 'NONE',  ( -165.7021400752470015, 1.848645179581459796, -200.5941117395221056 ) ) ;
#2366 = STYLED_ITEM ( 'NONE', ( #10905 ), #1525 ) ;
#2367 = CIRCLE ( 'NONE', #11688, 5.500000000000005329 ) ;
#2368 = DIRECTION ( 'NONE',  ( 1.000000000000000000, 0.000000000000000000, 0.000000000000000000 ) ) ;
#2369 = EDGE_CURVE ( 'NONE', #12890, #4958, #2126, .T. ) ;
#2370 = EDGE_CURVE ( 'NONE', #3500, #2835, #4666, .T. ) ;
#2371 = DIRECTION ( 'NONE',  ( 0.6368676505102716101, 0.000000000000000000, 0.7709731485165527420 ) ) ;
#2372 = FACE_OUTER_BOUND ( 'NONE', #6366, .T. ) ;
#2373 = CIRCLE ( 'NONE', #6848, 3.350000000000000089 ) ;
#2374 = ORIENTED_EDGE ( 'NONE', *, *, #9725, .T. ) ;
#2375 = CARTESIAN_POINT ( 'NONE',  ( 0.000000000000000000, 3.327561323230765034, 0.000000000000000000 ) ) ;
#2376 = CARTESIAN_POINT ( 'NONE',  ( 182.4625818711949137, -30.00000000000000000, 220.8838070499906223 ) ) ;
#2377 = ORIENTED_EDGE ( 'NONE', *, *, #2854, .T. ) ;
#2378 = CARTESIAN_POINT ( 'NONE',  ( -185.9653539489998195, -18.00000000000000000, -225.1241593668329699 ) ) ;
#2379 = DIRECTION ( 'NONE',  ( 0.000000000000000000, 0.000000000000000000, 1.000000000000000000 ) ) ;
#2380 = CARTESIAN_POINT ( 'NONE',  ( 211.9058003148608407, 20.08915143297736705, -151.8458048843642132 ) ) ;
#2381 = ORIENTED_EDGE ( 'NONE', *, *, #4479, .T. ) ;
#2382 = DIRECTION ( 'NONE',  ( 0.000000000000000000, -1.000000000000000000, 0.000000000000000000 ) ) ;
#2383 = CARTESIAN_POINT ( 'NONE',  ( -240.2579444297316797, 3.284593558773872157, -11.55663755354172295 ) ) ;
#2384 = CARTESIAN_POINT ( 'NONE',  ( -239.4103023865795592, 1.739665387982153755, 11.87322930970978518 ) ) ;
#2385 = LINE ( 'NONE', #1325, #10371 ) ;
#2386 = CONICAL_SURFACE ( 'NONE', #894, 6.500000000000005329, 0.7853981633974518317 ) ;
#2387 = CARTESIAN_POINT ( 'NONE',  ( 239.4650615381681860, -1.481238645317465075, 3.171113114088393026 ) ) ;
#2388 = CARTESIAN_POINT ( 'NONE',  ( -138.9238112054132444, -25.00000000000000000, 212.6409525001303678 ) ) ;
#2389 = ADVANCED_FACE ( 'NONE', ( #3309 ), #10451, .F. ) ;
#2390 = AXIS2_PLACEMENT_3D ( 'NONE', #7, #11333, #11133 ) ;
#2391 = ADVANCED_FACE ( 'NONE', ( #5645 ), #3369, .F. ) ;
#2392 = DIRECTION ( 'NONE',  ( -0.4503334343941556295, 0.7071067811865489050, -0.5451603414287969906 ) ) ;
#2393 = ORIENTED_EDGE ( 'NONE', *, *, #117, .T. ) ;
#2394 = VECTOR ( 'NONE', #10876, 1000.000000000000114 ) ;
#2395 = CARTESIAN_POINT ( 'NONE',  ( -1.009183486025028462E-12, 20.55460285106647689, 261.3381329044966606 ) ) ;
#2396 = DIRECTION ( 'NONE',  ( 0.000000000000000000, 0.000000000000000000, -1.000000000000000000 ) ) ;
#2397 = CARTESIAN_POINT ( 'NONE',  ( 197.8197553893915028, 30.00000000000000000, -70.77553482998990830 ) ) ;
#2398 = PRESENTATION_LAYER_ASSIGNMENT (  '', '', ( #4519 ) ) ;
#2399 = CARTESIAN_POINT ( 'NONE',  ( -197.8197553893909912, 29.00000000000000000, 69.77553482999131518 ) ) ;
#2400 = FACE_BOUND ( 'NONE', #7484, .T. ) ;
#2401 = DIRECTION ( 'NONE',  ( 0.000000000000000000, 0.000000000000000000, 1.000000000000000000 ) ) ;
#2402 = DIRECTION ( 'NONE',  ( -0.3518698652246392000, 0.5538822189107470706, 0.7545873610930026176 ) ) ;
#2403 = AXIS2_PLACEMENT_3D ( 'NONE', #7014, #10076, #11206 ) ;
#2404 = AXIS2_PLACEMENT_3D ( 'NONE', #10878, #9882, #1753 ) ;
#2405 = CLOSED_SHELL ( 'NONE', ( #12989, #496, #11197, #7786 ) ) ;
#2406 = CARTESIAN_POINT ( 'NONE',  ( 0.000000000000000000, 19.00000000000000000, 0.000000000000000000 ) ) ;
#2407 = ADVANCED_FACE ( 'NONE', ( #8462 ), #11533, .T. ) ;
#2408 = CARTESIAN_POINT ( 'NONE',  ( 31.19222893192144852, -29.00000000000000000, -286.4438302234616458 ) ) ;
#2409 = ORIENTED_EDGE ( 'NONE', *, *, #2466, .T. ) ;
#2410 = EDGE_LOOP ( 'NONE', ( #5759, #9455, #2377, #3932 ) ) ;
#2411 = DIRECTION ( 'NONE',  ( 0.000000000000000000, 0.01970892327970883220, 0.9998057603070481525 ) ) ;
#2412 = DIRECTION ( 'NONE',  ( 0.5469441386039890496, 0.000000000000000000, -0.8371691043312220470 ) ) ;
#2413 = AXIS2_PLACEMENT_3D ( 'NONE', #8506, #3492, #5495 ) ;
#2414 = AXIS2_PLACEMENT_3D ( 'NONE', #4823, #12966, #774 ) ;
#2415 = EDGE_CURVE ( 'NONE', #9966, #3848, #8124, .T. ) ;
#2416 = CIRCLE ( 'NONE', #3254, 239.0000000000000000 ) ;
#2417 = CARTESIAN_POINT ( 'NONE',  ( 207.6469600143036587, 19.96883745899249618, -159.3024069668460072 ) ) ;
#2418 = FACE_OUTER_BOUND ( 'NONE', #3802, .T. ) ;
#2419 = CARTESIAN_POINT ( 'NONE',  ( 0.000000000000000000, 0.000000000000000000, 0.000000000000000000 ) ) ;
#2420 = CARTESIAN_POINT ( 'NONE',  ( -240.6986105847286694, 4.249529545457076729, 10.95469206492581371 ) ) ;
#2421 = DIRECTION ( 'NONE',  ( 0.6368676505102695007, 0.000000000000000000, 0.7709731485165545184 ) ) ;
#2422 = ORIENTED_EDGE ( 'NONE', *, *, #5347, .F. ) ;
#2423 = CARTESIAN_POINT ( 'NONE',  ( 130.4544329367270450, 20.79694577634646535, -225.9597979674043984 ) ) ;
#2424 = VECTOR ( 'NONE', #209, 1000.000000000000114 ) ;
#2425 = VERTEX_POINT ( 'NONE', #7452 ) ;
#2426 = FACE_OUTER_BOUND ( 'NONE', #1855, .T. ) ;
#2427 = VERTEX_POINT ( 'NONE', #6588 ) ;
#2428 = EDGE_LOOP ( 'NONE', ( #5143, #2422, #4815, #3360, #6172, #5954 ) ) ;
#2429 = CIRCLE ( 'NONE', #2002, 249.7999999999999829 ) ;
#2430 = DIRECTION ( 'NONE',  ( 0.000000000000000000, 0.000000000000000000, 1.000000000000000000 ) ) ;
#2431 = DIRECTION ( 'NONE',  ( -0.4503334343941563511, -0.7071067811865480168, -0.5451603414287977678 ) ) ;
#2432 = DIRECTION ( 'NONE',  ( 0.000000000000000000, 1.000000000000000000, 0.000000000000000000 ) ) ;
#2433 = AXIS2_PLACEMENT_3D ( 'NONE', #11709, #10824, #2682 ) ;
#2434 = CARTESIAN_POINT ( 'NONE',  ( -238.7984600057413616, 0.6745672505613249381, -11.73164896005920710 ) ) ;
#2435 = CARTESIAN_POINT ( 'NONE',  ( -225.1241593668336236, -18.00000000000000000, 185.9653539489990521 ) ) ;
#2436 = B_SPLINE_CURVE_WITH_KNOTS ( 'NONE', 3,
 ( #1789, #6411, #12912, #4910, #12113, #724, #3773, #11914, #2764, #785, #2968, #8918, #1917, #11984, #6922, #10981, #1853, #8982, #10045, #3910, #6983, #1112, #495, #6183, #1044, #2357, #11630, #10558, #6433, #7118, #5551, #4356, #7177, #4411, #9609, #10236, #5102, #11564, #5168, #2484, #8435, #4544, #7494, #8496, #1362, #8626, #1488, #3034, #9247, #6500, #2043, #12489, #1425, #53, #6112, #3342, #10165, #9544, #6563, #302, #10618, #8562, #5486, #11176, #7421, #7557 ),
 .UNSPECIFIED., .F., .F.,
 ( 4, 2, 2, 2, 2, 2, 2, 2, 2, 2, 2, 2, 2, 2, 2, 2, 2, 2, 2, 2, 2, 2, 2, 2, 2, 2, 2, 2, 2, 2, 2, 2, 4 ),
 ( 0.5000000000000000000, 0.5156250000000000000, 0.5312500000000000000, 0.5468749999999998890, 0.5624999999999998890, 0.5781249999999998890, 0.5937499999999998890, 0.6093749999999998890, 0.6249999999999998890, 0.6406249999999998890, 0.6562499999999998890, 0.6718749999999998890, 0.6874999999999998890, 0.7031249999999998890, 0.7187499999999998890, 0.7343749999999998890, 0.7499999999999998890, 0.7656249999999998890, 0.7812500000000000000, 0.7968750000000000000, 0.8125000000000000000, 0.8281250000000000000, 0.8437500000000000000, 0.8593750000000000000, 0.8750000000000001110, 0.8906250000000001110, 0.9062500000000002220, 0.9218750000000002220, 0.9375000000000002220, 0.9531250000000001110, 0.9687500000000001110, 0.9843750000000000000, 1.000000000000000000 ),
 .UNSPECIFIED. ) ;
#2437 = CONTEXT_DEPENDENT_SHAPE_REPRESENTATION ( #8646, #5325 ) ;
#2438 = VERTEX_POINT ( 'NONE', #11526 ) ;
#2439 = CARTESIAN_POINT ( 'NONE',  ( 197.8197553893920144, 30.00000000000000000, 64.27553482998850143 ) ) ;
#2440 = EDGE_LOOP ( 'NONE', ( #9151, #9297, #2088, #9387 ) ) ;
#2441 = CARTESIAN_POINT ( 'NONE',  ( -244.0876578025649621, 8.170278137860064405, -8.444514117778142648 ) ) ;
#2442 = CARTESIAN_POINT ( 'NONE',  ( 71.82423009839129691, 18.00000000000000000, 190.8354503650405150 ) ) ;
#2443 = ADVANCED_FACE ( 'NONE', ( #11591 ), #5, .F. ) ;
#2444 = CIRCLE ( 'NONE', #12655, 0.7999999999999999334 ) ;
#2445 = CARTESIAN_POINT ( 'NONE',  ( 0.000000000000000000, 0.000000000000000000, 0.000000000000000000 ) ) ;
#2446 = DIRECTION ( 'NONE',  ( 0.000000000000000000, -1.000000000000000000, 0.000000000000000000 ) ) ;
#2447 = CARTESIAN_POINT ( 'NONE',  ( -238.6985546758615442, -1.431921744593627863E-13, 12.00000000011287504 ) ) ;
#2448 = CARTESIAN_POINT ( 'NONE',  ( -240.8352866738073601, -4.521734056337656682, -10.84609021955956898 ) ) ;
#2449 = VECTOR ( 'NONE', #3995, 1000.000000000000000 ) ;
#2450 = CARTESIAN_POINT ( 'NONE',  ( 197.8197553893920144, 18.00000000000000000, 57.77553482998850853 ) ) ;
#2451 = PRODUCT_DEFINITION_SHAPE ( 'NONE', 'NONE',  #13057 ) ;
#2452 = DIRECTION ( 'NONE',  ( 0.000000000000000000, 0.000000000000000000, 1.000000000000000000 ) ) ;
#2453 = AXIS2_PLACEMENT_3D ( 'NONE', #8178, #3090, #6372 ) ;
#2454 = CARTESIAN_POINT ( 'NONE',  ( -229.8611669809016007, 8.953871400566880467, 7.991408290370279666 ) ) ;
#2455 = CONTEXT_DEPENDENT_SHAPE_REPRESENTATION ( #1282, #6650 ) ;
#2456 = EDGE_CURVE ( 'NONE', #6913, #8118, #7451, .T. ) ;
#2457 = DIRECTION ( 'NONE',  ( -1.000000000000000000, 0.000000000000000000, 0.000000000000000000 ) ) ;
#2458 = ORIENTED_EDGE ( 'NONE', *, *, #4437, .F. ) ;
#2459 = CIRCLE ( 'NONE', #5008, 249.0000000000000284 ) ;
#2460 = CARTESIAN_POINT ( 'NONE',  ( -115.7315435904061331, 19.96883746069636700, -234.7354397749499810 ) ) ;
#2461 = FACE_OUTER_BOUND ( 'NONE', #4092, .T. ) ;
#2462 = CARTESIAN_POINT ( 'NONE',  ( 27.68945685411497593, -30.00000000000000000, -290.6841825403026291 ) ) ;
#2463 =( REPRESENTATION_RELATIONSHIP ('NONE','NONE', #12019, #5191 ) REPRESENTATION_RELATIONSHIP_WITH_TRANSFORMATION ( #3316 )SHAPE_REPRESENTATION_RELATIONSHIP( ) );
#2464 = CARTESIAN_POINT ( 'NONE',  ( -7.780566028168587395E-13, 20.08915143297736350, 260.5542428351130866 ) ) ;
#2465 = CARTESIAN_POINT ( 'NONE',  ( -59.19439222780491150, 20.08915143297736705, 253.8843055347117001 ) ) ;
#2466 = EDGE_CURVE ( 'NONE', #11681, #431, #10518, .T. ) ;
#2467 = EDGE_CURVE ( 'NONE', #4948, #11098, #3421, .T. ) ;
#2468 = CARTESIAN_POINT ( 'NONE',  ( 226.7234983661818717, -3.822755691033211001, 0.07535703595917145337 ) ) ;
#2469 = CARTESIAN_POINT ( 'NONE',  ( -41.69198534955602042, -138.4705547276867321, -3.647576077975211994 ) ) ;
#2470 = CARTESIAN_POINT ( 'NONE',  ( -136.1890905123932782, -22.00000000000000000, 208.4551069784743049 ) ) ;
#2471 = CARTESIAN_POINT ( 'NONE',  ( -242.0646888574074467, -6.354939414423857791, -10.17926273101336143 ) ) ;
#2472 = DIRECTION ( 'NONE',  ( 0.6368676505102696117, 0.000000000000000000, 0.7709731485165545184 ) ) ;
#2473 = ORIENTED_EDGE ( 'NONE', *, *, #2854, .F. ) ;
#2474 = ORIENTED_EDGE ( 'NONE', *, *, #938, .F. ) ;
#2475 = CARTESIAN_POINT ( 'NONE',  ( 235.0999999999999943, -2.749465840844381948, 0.05419953901920007699 ) ) ;
#2476 = CARTESIAN_POINT ( 'NONE',  ( 197.8197553893915028, 19.00000000000000000, -64.27553482998990830 ) ) ;
#2477 = ADVANCED_FACE ( 'NONE', ( #7641 ), #11719, .T. ) ;
#2478 = CARTESIAN_POINT ( 'NONE',  ( -67.76049180359858326, 20.55460285124812359, -252.9796497731095997 ) ) ;
#2479 = EDGE_CURVE ( 'NONE', #11054, #11150, #8522, .T. ) ;
#2480 = CARTESIAN_POINT ( 'NONE',  ( 0.000000000000000000, 0.000000000000000000, 0.000000000000000000 ) ) ;
#2481 = PRODUCT_DEFINITION_SHAPE ( 'NONE', 'NONE',  #13184 ) ;
#2482 = DIRECTION ( 'NONE',  ( -1.000000000000000000, 0.000000000000000000, -3.491481338843133355E-15 ) ) ;
#2483 = DIRECTION ( 'NONE',  ( 0.6368676505102707219, 0.000000000000000000, 0.7709731485165535192 ) ) ;
#2484 = CARTESIAN_POINT ( 'NONE',  ( -247.0684411393756648, 20.79694577634646535, 83.86521783953146780 ) ) ;
#2485 = ORIENTED_EDGE ( 'NONE', *, *, #2315, .F. ) ;
#2486 = CARTESIAN_POINT ( 'NONE',  ( 257.4287020129720531, 20.79694577634646890, -42.50473797389749109 ) ) ;
#2487 = EDGE_CURVE ( 'NONE', #9382, #4412, #7903, .T. ) ;
#2488 = ORIENTED_EDGE ( 'NONE', *, *, #1988, .F. ) ;
#2489 = AXIS2_PLACEMENT_3D ( 'NONE', #6494, #291, #9536 ) ;
#2490 = DIRECTION ( 'NONE',  ( 0.6368676505102696117, 0.000000000000000000, 0.7709731485165545184 ) ) ;
#2491 = ORIENTED_EDGE ( 'NONE', *, *, #3333, .T. ) ;
#2492 = VERTEX_POINT ( 'NONE', #6844 ) ;
#2493 = CARTESIAN_POINT ( 'NONE',  ( -190.1049936773165996, -30.00000000000000000, -230.1354848321905706 ) ) ;
#2494 = AXIS2_PLACEMENT_3D ( 'NONE', #3572, #10714, #11722 ) ;
#2495 = CARTESIAN_POINT ( 'NONE',  ( 235.4000000000000057, 4.550331206106116078, 2.508881407069060376 ) ) ;
#2496 = CARTESIAN_POINT ( 'NONE',  ( 239.4667603743168058, 1.483520951545550526, -3.170043417372648165 ) ) ;
#2497 = FACE_OUTER_BOUND ( 'NONE', #1014, .T. ) ;
#2498 = CARTESIAN_POINT ( 'NONE',  ( -249.7800409167776934, 11.57739048715638397, -3.170426907196378430 ) ) ;
#2499 = EDGE_LOOP ( 'NONE', ( #4914, #8787, #7367, #4008 ) ) ;
#2500 = CARTESIAN_POINT ( 'NONE',  ( -238.8666832504503930, -0.8657828299950671713, 11.71814331008092402 ) ) ;
#2502 = ORIENTED_EDGE ( 'NONE', *, *, #12791, .F. ) ;
#2501 =( GEOMETRIC_REPRESENTATION_CONTEXT ( 3 ) GLOBAL_UNCERTAINTY_ASSIGNED_CONTEXT ( ( #1824 ) ) GLOBAL_UNIT_ASSIGNED_CONTEXT ( ( #12896, #6905, #9095 ) ) REPRESENTATION_CONTEXT ( 'NONE', 'WORKASPACE' ) );
#2503 =( REPRESENTATION_RELATIONSHIP ('NONE','NONE', #12019, #182 ) REPRESENTATION_RELATIONSHIP_WITH_TRANSFORMATION ( #1918 )SHAPE_REPRESENTATION_RELATIONSHIP( ) );
#2504 = CARTESIAN_POINT ( 'NONE',  ( -240.1208361041844910, 2.772967769358964940, -11.41810622433052025 ) ) ;
#2505 = CARTESIAN_POINT ( 'NONE',  ( -122.2593324768359935, 18.00000000000000000, -161.7755348299880040 ) ) ;
#2506 = CARTESIAN_POINT ( 'NONE',  ( 0.000000000000000000, 0.000000000000000000, -250.0000000000000000 ) ) ;
#2507 = DIRECTION ( 'NONE',  ( 0.000000000000000000, 0.000000000000000000, 1.000000000000000000 ) ) ;
#2508 = CARTESIAN_POINT ( 'NONE',  ( -239.0092219884379858, 1.200944422457546068, 11.93976291956724900 ) ) ;
#2509 = CARTESIAN_POINT ( 'NONE',  ( -229.8692747951969579, 8.832110811273086171, 7.759242523040085437 ) ) ;
#2510 = AXIS2_PLACEMENT_3D ( 'NONE', #13012, #2866, #3676 ) ;
#2511 = CARTESIAN_POINT ( 'NONE',  ( -246.3126759746303946, -9.340233780147908504, 7.533927936259328995 ) ) ;
#2512 = EDGE_CURVE ( 'NONE', #4880, #1904, #11920, .T. ) ;
#2513 = DIRECTION ( 'NONE',  ( 0.000000000000000000, -0.8757116489157734662, -0.4828344519120573719 ) ) ;
#2514 = CARTESIAN_POINT ( 'NONE',  ( 7.267391899529532573, -138.4705547276867321, 41.21542755584205509 ) ) ;
#2515 =( REPRESENTATION_RELATIONSHIP ('NONE','NONE', #12019, #182 ) REPRESENTATION_RELATIONSHIP_WITH_TRANSFORMATION ( #7083 )SHAPE_REPRESENTATION_RELATIONSHIP( ) );
#2516 = CARTESIAN_POINT ( 'NONE',  ( -229.9813512810838461, 11.63766203094939300, 2.950567834083252627 ) ) ;
#2517 = CONTEXT_DEPENDENT_SHAPE_REPRESENTATION ( #12265, #8771 ) ;
#2518 = CIRCLE ( 'NONE', #1455, 6.500000000000005329 ) ;
#2519 = VECTOR ( 'NONE', #5676, 1000.000000000000000 ) ;
#2520 = ORIENTED_EDGE ( 'NONE', *, *, #738, .T. ) ;
#2521 = AXIS2_PLACEMENT_3D ( 'NONE', #7016, #4671, #8016 ) ;
#2522 = CARTESIAN_POINT ( 'NONE',  ( -0.000000000000000000, -30.00000000000000000, 0.000000000000000000 ) ) ;
#2523 = ORIENTED_EDGE ( 'NONE', *, *, #5493, .T. ) ;
#2524 = CARTESIAN_POINT ( 'NONE',  ( -261.1558126970361400, 19.96883746064829168, 17.09264059829825300 ) ) ;
#2525 = DIRECTION ( 'NONE',  ( -1.000000000000000000, 0.000000000000000000, 0.000000000000000000 ) ) ;
#2526 = DIRECTION ( 'NONE',  ( -0.000000000000000000, -1.000000000000000000, 0.000000000000000000 ) ) ;
#2527 = CARTESIAN_POINT ( 'NONE',  ( 0.000000000000000000, 30.00000000000000000, 0.000000000000000000 ) ) ;
#2528 = FACE_OUTER_BOUND ( 'NONE', #3079, .T. ) ;
#2529 = EDGE_CURVE ( 'NONE', #4415, #6490, #465, .T. ) ;
#2530 = EDGE_CURVE ( 'NONE', #6733, #4344, #9836, .T. ) ;
#2531 = CONICAL_SURFACE ( 'NONE', #9548, 305.0000000000000000, 0.7853981633974758125 ) ;
#2532 = CYLINDRICAL_SURFACE ( 'NONE', #6653, 245.7999999999999829 ) ;
#2533 = DIRECTION ( 'NONE',  ( 0.5735764363510443831, 0.000000000000000000, 0.8191520442889930198 ) ) ;
#2534 = CARTESIAN_POINT ( 'NONE',  ( 229.9832014715669004, 2.135344109160686177, -2.782701128735099338 ) ) ;
#2535 = VECTOR ( 'NONE', #12221, 1000.000000000000000 ) ;
#2536 = CARTESIAN_POINT ( 'NONE',  ( -240.9204428195482137, -4.702057767565119839, -11.04114865042053317 ) ) ;
#2537 = DIRECTION ( 'NONE',  ( 0.000000000000000000, 0.000000000000000000, 1.000000000000000000 ) ) ;
#2538 = EDGE_LOOP ( 'NONE', ( #5365, #3282, #8439, #7987 ) ) ;
#2539 = VERTEX_POINT ( 'NONE', #11975 ) ;
#2540 = EDGE_CURVE ( 'NONE', #5028, #9692, #5348, .T. ) ;
#2541 = AXIS2_PLACEMENT_3D ( 'NONE', #1373, #4367, #440 ) ;
#2542 = DIRECTION ( 'NONE',  ( 0.5469441386039890496, 0.000000000000000000, -0.8371691043312220470 ) ) ;
#2543 = FACE_BOUND ( 'NONE', #10166, .T. ) ;
#2544 = CARTESIAN_POINT ( 'NONE',  ( 84.20717312453921011, 20.55460285117019126, -247.9906035365278001 ) ) ;
#2545 = DIRECTION ( 'NONE',  ( 0.000000000000000000, 0.000000000000000000, -1.000000000000000000 ) ) ;
#2546 = DIRECTION ( 'NONE',  ( 0.1736481776669273613, 0.000000000000000000, 0.9848077530122085754 ) ) ;
#2547 = CARTESIAN_POINT ( 'NONE',  ( -240.9194688703003067, 4.677296208860544979, 10.77948277563700330 ) ) ;
#2548 = DIRECTION ( 'NONE',  ( 0.000000000000000000, 0.000000000000000000, -1.000000000000000000 ) ) ;
#2549 = AXIS2_PLACEMENT_3D ( 'NONE', #1601, #598, #3656 ) ;
#2550 = ORIENTED_EDGE ( 'NONE', *, *, #956, .F. ) ;
#2551 = ORIENTED_EDGE ( 'NONE', *, *, #554, .F. ) ;
#2552 = DIRECTION ( 'NONE',  ( 0.000000000000000000, 1.000000000000000000, 0.000000000000000000 ) ) ;
#2553 = ORIENTED_EDGE ( 'NONE', *, *, #6938, .T. ) ;
#2554 = EDGE_LOOP ( 'NONE', ( #4704, #6063, #1692, #10918 ) ) ;
#2555 = EDGE_CURVE ( 'NONE', #1760, #9966, #4072, .T. ) ;
#2556 = EDGE_CURVE ( 'NONE', #10957, #327, #9818, .T. ) ;
#2557 = CARTESIAN_POINT ( 'NONE',  ( 224.4939760857161843, 0.000000000000000000, 0.000000000000000000 ) ) ;
#2558 = CARTESIAN_POINT ( 'NONE',  ( -225.1241593668336236, -30.00000000000000000, 185.9653539489990521 ) ) ;
#2559 = DIRECTION ( 'NONE',  ( 0.000000000000000000, -1.000000000000000000, -0.000000000000000000 ) ) ;
#2560 = AXIS2_PLACEMENT_3D ( 'NONE', #12864, #2655, #1808 ) ;
#2561 = CARTESIAN_POINT ( 'NONE',  ( 220.3999999999999773, -2.249562960690858038, 0.04434507737934551691 ) ) ;
#2562 =( LENGTH_UNIT ( ) NAMED_UNIT ( * ) SI_UNIT ( .MILLI., .METRE. ) );
#2563 = CARTESIAN_POINT ( 'NONE',  ( 122.2593324768334071, 19.00000000000000000, -173.7755348299895104 ) ) ;
#2564 = EDGE_LOOP ( 'NONE', ( #2822, #4515, #8322, #1744 ) ) ;
#2565 = LINE ( 'NONE', #5444, #9447 ) ;
#2566 = ORIENTED_EDGE ( 'NONE', *, *, #1850, .F. ) ;
#2567 = CARTESIAN_POINT ( 'NONE',  ( -244.1927368939279859, 8.241533436879795005, -8.374943116871326865 ) ) ;
#2568 = CARTESIAN_POINT ( 'NONE',  ( -171.3173979872628649, 20.00000000000000000, -207.3917769509529023 ) ) ;
#2569 = ORIENTED_EDGE ( 'NONE', *, *, #4322, .F. ) ;
#2570 = EDGE_CURVE ( 'NONE', #4210, #8008, #879, .T. ) ;
#2571 = DIRECTION ( 'NONE',  ( 0.000000000000000000, 0.9998057603070481525, -0.01970892327970899874 ) ) ;
#2572 = DIRECTION ( 'NONE',  ( 0.000000000000000000, 0.000000000000000000, 1.000000000000000000 ) ) ;
#2573 = CARTESIAN_POINT ( 'NONE',  ( 159.3442861576696998, -29.00000000000000000, 192.8974817588416784 ) ) ;
#2574 = DIRECTION ( 'NONE',  ( 0.4503334343941562956, -0.7071067811865480168, 0.5451603414287978788 ) ) ;
#2575 = CIRCLE ( 'NONE', #12592, 6.500000000000005329 ) ;
#2576 = DIRECTION ( 'NONE',  ( -0.6368676505102707219, 0.000000000000000000, -0.7709731485165536302 ) ) ;
#2577 = AXIS2_PLACEMENT_3D ( 'NONE', #4768, #11787, #6782 ) ;
#2578 = EDGE_CURVE ( 'NONE', #11921, #2857, #6982, .T. ) ;
#2579 = DIRECTION ( 'NONE',  ( -0.6368676505102708330, 0.000000000000000000, -0.7709731485165536302 ) ) ;
#2580 = CARTESIAN_POINT ( 'NONE',  ( -122.2593324768321992, 18.00000000000000000, 168.2755348299905052 ) ) ;
#2581 = ORIENTED_EDGE ( 'NONE', *, *, #5256, .F. ) ;
#2582 = ORIENTED_EDGE ( 'NONE', *, *, #4322, .T. ) ;
#2583 = CARTESIAN_POINT ( 'NONE',  ( 235.4000000000000057, -4.550331206106116078, -2.508881407069070590 ) ) ;
#2584 = ORIENTED_EDGE ( 'NONE', *, *, #9641, .T. ) ;
#2585 = CARTESIAN_POINT ( 'NONE',  ( 196.7513681799443361, 19.96883746182971464, 172.5787240285351345 ) ) ;
#2586 = DIRECTION ( 'NONE',  ( 0.000000000000000000, -1.000000000000000000, 0.000000000000000000 ) ) ;
#2587 = CARTESIAN_POINT ( 'NONE',  ( 220.3999999999999773, -0.01970892327970899874, -0.9998057603070481525 ) ) ;
#2588 = CIRCLE ( 'NONE', #9201, 6.500000000000005329 ) ;
#2589 = CARTESIAN_POINT ( 'NONE',  ( -290.6841825403030839, -29.00000000000000000, -27.68945685411394919 ) ) ;
#2590 = CARTESIAN_POINT ( 'NONE',  ( 235.4000000000000057, -2.999417280921144346, 0.05912676983912736745 ) ) ;
#2591 = CARTESIAN_POINT ( 'NONE',  ( -27.68945685411286561, -19.00000000000000000, 290.6841825403027997 ) ) ;
#2592 = DIRECTION ( 'NONE',  ( -0.8660254037844415942, 0.000000000000000000, 0.4999999999999949485 ) ) ;
#2593 = DIRECTION ( 'NONE',  ( 0.6368676505102707219, 0.000000000000000000, 0.7709731485165535192 ) ) ;
#2594 = AXIS2_PLACEMENT_3D ( 'NONE', #7268, #5261, #10257 ) ;
#2595 = AXIS2_PLACEMENT_3D ( 'NONE', #2779, #11221, #7231 ) ;
#2596 = CARTESIAN_POINT ( 'NONE',  ( -240.4621951198754175, -3.755930367947129422, -11.39707303937288785 ) ) ;
#2597 = DIRECTION ( 'NONE',  ( 0.000000000000000000, -1.000000000000000000, 0.000000000000000000 ) ) ;
#2598 = TOROIDAL_SURFACE ( 'NONE', #5150, 238.4705882352940307, 2.000000000000000000 ) ;
#2599 = EDGE_LOOP ( 'NONE', ( #11147, #11321, #6390, #12753, #2243, #12299 ) ) ;
#2600 = ADVANCED_FACE ( 'NONE', ( #780, #2755 ), #3903, .F. ) ;
#2601 = VERTEX_POINT ( 'NONE', #1639 ) ;
#2602 = EDGE_CURVE ( 'NONE', #11697, #2539, #3635, .T. ) ;
#2603 = DIRECTION ( 'NONE',  ( 0.000000000000000000, 0.7071067811865480168, 0.7071067811865470176 ) ) ;
#2604 = DIRECTION ( 'NONE',  ( 8.659560562354572940E-17, -0.7071067811865771047, 0.7071067811865180408 ) ) ;
#2605 = CARTESIAN_POINT ( 'NONE',  ( 17.10461161519311091, 20.55460285116648933, 261.3381329044966606 ) ) ;
#2606 = FACE_OUTER_BOUND ( 'NONE', #9434, .T. ) ;
#2607 = CARTESIAN_POINT ( 'NONE',  ( 0.000000000000000000, 0.000000000000000000, 0.000000000000000000 ) ) ;
#2608 = CIRCLE ( 'NONE', #3036, 2.000000000000001776 ) ;
#2609 = DIRECTION ( 'NONE',  ( 0.9135454576426033091, 0.4066576386751313277, -0.008016341293427218032 ) ) ;
#2610 = CARTESIAN_POINT ( 'NONE',  ( 0.000000000000000000, 3.327561323230709966, 0.000000000000000000 ) ) ;
#2611 = ORIENTED_EDGE ( 'NONE', *, *, #6441, .T. ) ;
#2612 = FACE_OUTER_BOUND ( 'NONE', #4380, .T. ) ;
#2613 = EDGE_LOOP ( 'NONE', ( #11994, #8541, #5920, #5414 ) ) ;
#2614 = ORIENTED_EDGE ( 'NONE', *, *, #2081, .F. ) ;
#2615 = VECTOR ( 'NONE', #10566, 1000.000000000000000 ) ;
#2616 = CONICAL_SURFACE ( 'NONE', #7732, 6.500000000000005329, 0.7853981633974476129 ) ;
#2617 = CARTESIAN_POINT ( 'NONE',  ( 115.3046144132256785, 20.08915143297736705, -233.8077470125390676 ) ) ;
#2618 = VERTEX_POINT ( 'NONE', #9766 ) ;
#2619 = DIRECTION ( 'NONE',  ( 0.000000000000000000, 1.000000000000000000, 0.000000000000000000 ) ) ;
#2620 = CARTESIAN_POINT ( 'NONE',  ( -240.0943994960963721, 2.684989249075541817, -11.43947242957938037 ) ) ;
#2621 = CARTESIAN_POINT ( 'NONE',  ( 130.5770120857756069, 20.08915143320244567, -226.1171533158560010 ) ) ;
#2622 = DIRECTION ( 'NONE',  ( -0.000000000000000000, -1.000000000000000000, 0.000000000000000000 ) ) ;
#2623 = CARTESIAN_POINT ( 'NONE',  ( -136.1890905123932782, -22.00000000000000000, 208.4551069784743049 ) ) ;
#2624 = EDGE_CURVE ( 'NONE', #379, #12401, #2373, .T. ) ;
#2625 = TOROIDAL_SURFACE ( 'NONE', #513, 247.7999999999999829, 2.000000000000000000 ) ;
#2626 = EDGE_CURVE ( 'NONE', #8550, #11184, #2575, .T. ) ;
#2627 = ORIENTED_EDGE ( 'NONE', *, *, #12425, .F. ) ;
#2628 = FACE_OUTER_BOUND ( 'NONE', #3601, .T. ) ;
#2629 = ORIENTED_EDGE ( 'NONE', *, *, #10487, .F. ) ;
#2630 =( REPRESENTATION_RELATIONSHIP ('NONE','NONE', #12019, #5191 ) REPRESENTATION_RELATIONSHIP_WITH_TRANSFORMATION ( #529 )SHAPE_REPRESENTATION_RELATIONSHIP( ) );
#2631 = CARTESIAN_POINT ( 'NONE',  ( -242.6830939082452403, 7.008887184829689865, -9.430537149009394327 ) ) ;
#2632 = ORIENTED_EDGE ( 'NONE', *, *, #11572, .T. ) ;
#2633 = CARTESIAN_POINT ( 'NONE',  ( 235.4000000000000057, 2.749465840844381948, -0.05419953901919974393 ) ) ;
#2634 = DIRECTION ( 'NONE',  ( 0.6368676505102709440, 0.000000000000000000, 0.7709731485165532971 ) ) ;
#2635 = CARTESIAN_POINT ( 'NONE',  ( -159.3442861576697283, -25.50000000000000000, -192.8974817588417068 ) ) ;
#2636 = CARTESIAN_POINT ( 'NONE',  ( 0.000000000000000000, 0.000000000000000000, 250.0000000000000000 ) ) ;
#2637 = CARTESIAN_POINT ( 'NONE',  ( -244.1671264040621168, -8.232476464565948504, 8.730683391379466585 ) ) ;
#2638 = EDGE_CURVE ( 'NONE', #6987, #5762, #8775, .T. ) ;
#2639 = DIRECTION ( 'NONE',  ( 0.000000000000000000, 0.000000000000000000, 1.000000000000000000 ) ) ;
#2640 = VERTEX_POINT ( 'NONE', #7773 ) ;
#2641 = DIRECTION ( 'NONE',  ( 0.000000000000000000, 0.000000000000000000, 1.000000000000000000 ) ) ;
#2642 = AXIS2_PLACEMENT_3D ( 'NONE', #10598, #9474, #10475 ) ;
#2643 = ORIENTED_EDGE ( 'NONE', *, *, #2109, .T. ) ;
#2644 = ADVANCED_FACE ( 'NONE', ( #5849 ), #9397, .F. ) ;
#2645 = ORIENTED_EDGE ( 'NONE', *, *, #8234, .T. ) ;
#2646 = CARTESIAN_POINT ( 'NONE',  ( 3.010181832304193602E-14, 25.00000000000000000, 245.7999999999999829 ) ) ;
#2647 = ORIENTED_EDGE ( 'NONE', *, *, #9123, .F. ) ;
#2648 = CARTESIAN_POINT ( 'NONE',  ( -115.8123742918135832, 20.55460285136280518, 234.8993005745464586 ) ) ;
#2649 = CARTESIAN_POINT ( 'NONE',  ( -165.3358371128620661, -2.772967769358684720, -200.1506762031204971 ) ) ;
#2650 = LINE ( 'NONE', #11999, #2940 ) ;
#2651 = DIRECTION ( 'NONE',  ( 1.000000000000000000, 0.000000000000000000, 0.000000000000000000 ) ) ;
#2652 = MECHANICAL_DESIGN_GEOMETRIC_PRESENTATION_REPRESENTATION (  '', ( #12459 ), #9051 ) ;
#2653 = CARTESIAN_POINT ( 'NONE',  ( -242.1349625647511346, 6.437046976376021412, 10.12773524473490916 ) ) ;
#2654 = DIRECTION ( 'NONE',  ( -1.000000000000000000, 0.000000000000000000, 0.000000000000000000 ) ) ;
#2655 = DIRECTION ( 'NONE',  ( 0.2847642722309917662, 0.5538822189107470706, -0.7823834078220606170 ) ) ;
#2656 = CARTESIAN_POINT ( 'NONE',  ( 229.9760364581192960, 1.127696253648076574, -3.321182350956919827 ) ) ;
#2657 = CARTESIAN_POINT ( 'NONE',  ( -249.6793054725033585, 11.18791971373266669, -3.590677820213459714 ) ) ;
#2658 = CARTESIAN_POINT ( 'NONE',  ( 130.7196491263533460, -20.69999999999999929, -200.0834159351620940 ) ) ;
#2659 = AXIS2_PLACEMENT_3D ( 'NONE', #10495, #429, #5428 ) ;
#2660 = AXIS2_PLACEMENT_3D ( 'NONE', #10499, #8438, #9435 ) ;
#2661 = CARTESIAN_POINT ( 'NONE',  ( -229.7228301394881953, -4.075732016279721037, -11.28829787118005257 ) ) ;
#2662 = EDGE_LOOP ( 'NONE', ( #2824, #6264, #2674, #3519 ) ) ;
#2663 = ORIENTED_EDGE ( 'NONE', *, *, #11525, .T. ) ;
#2664 = DIRECTION ( 'NONE',  ( -0.5469441386039890496, 0.000000000000000000, 0.8371691043312220470 ) ) ;
#2665 = CARTESIAN_POINT ( 'NONE',  ( 3.059167704270088292E-14, 29.00000000000000000, 249.7999999999999829 ) ) ;
#2666 = CARTESIAN_POINT ( 'NONE',  ( 196.8887528222392973, 20.55460285123310982, 172.6991790951400390 ) ) ;
#2667 = CARTESIAN_POINT ( 'NONE',  ( -197.8197553893924976, 30.00000000000000000, -64.27553482998719403 ) ) ;
#2668 = CARTESIAN_POINT ( 'NONE',  ( 0.000000000000000000, 0.000000000000000000, 0.000000000000000000 ) ) ;
#2669 = DIRECTION ( 'NONE',  ( -0.6368676505102707219, 0.000000000000000000, -0.7709731485165535192 ) ) ;
#2670 = DIRECTION ( 'NONE',  ( 0.000000000000000000, -1.000000000000000000, 0.000000000000000000 ) ) ;
#2671 = ADVANCED_FACE ( 'NONE', ( #8040 ), #4968, .F. ) ;
#2672 = VERTEX_POINT ( 'NONE', #1036 ) ;
#2673 = CARTESIAN_POINT ( 'NONE',  ( -159.3442861576697283, -21.50000000000000000, -192.8974817588416499 ) ) ;
#2674 = ORIENTED_EDGE ( 'NONE', *, *, #2074, .T. ) ;
#2675 = ORIENTED_EDGE ( 'NONE', *, *, #2168, .F. ) ;
#2676 = CARTESIAN_POINT ( 'NONE',  ( 253.8843055347118138, 20.08915143297736705, 59.19439222780464149 ) ) ;
#2677 = ORIENTED_EDGE ( 'NONE', *, *, #12177, .F. ) ;
#2678 = LINE ( 'NONE', #8759, #11140 ) ;
#2679 = CARTESIAN_POINT ( 'NONE',  ( 0.000000000000000000, 0.000000000000000000, 0.000000000000000000 ) ) ;
#2680 =( REPRESENTATION_RELATIONSHIP ('NONE','NONE', #12019, #182 ) REPRESENTATION_RELATIONSHIP_WITH_TRANSFORMATION ( #3130 )SHAPE_REPRESENTATION_RELATIONSHIP( ) );
#2681 = CARTESIAN_POINT ( 'NONE',  ( 135.8846079354933352, -28.60000000000000142, -256.1940150085812888 ) ) ;
#2682 = DIRECTION ( 'NONE',  ( 0.000000000000000000, -0.9998057603070481525, 0.01970892327970899874 ) ) ;
#2683 = LINE ( 'NONE', #2884, #9631 ) ;
#2684 = EDGE_CURVE ( 'NONE', #8633, #3549, #1097, .T. ) ;
#2685 = ORIENTED_EDGE ( 'NONE', *, *, #1829, .T. ) ;
#2686 = CARTESIAN_POINT ( 'NONE',  ( -238.7109915768028827, -0.1647346007394138723, 11.75000001785272907 ) ) ;
#2687 = ORIENTED_EDGE ( 'NONE', *, *, #9342, .T. ) ;
#2688 = PRODUCT_DEFINITION_SHAPE ( 'NONE', 'NONE',  #13178 ) ;
#2689 = CARTESIAN_POINT ( 'NONE',  ( -241.2291919109576668, 5.202024195572752419, -10.53597307948211537 ) ) ;
#2690 = VERTEX_POINT ( 'NONE', #5094 ) ;
#2691 = EDGE_CURVE ( 'NONE', #9851, #12208, #11743, .T. ) ;
#2692 = DIRECTION ( 'NONE',  ( 0.000000000000000000, 1.000000000000000000, 0.000000000000000000 ) ) ;
#2693 = CARTESIAN_POINT ( 'NONE',  ( 0.000000000000000000, 25.00000000000000000, 249.2999999999999829 ) ) ;
#2694 = CARTESIAN_POINT ( 'NONE',  ( 0.000000000000000000, 19.00000000000000000, 0.000000000000000000 ) ) ;
#2695 = FACE_OUTER_BOUND ( 'NONE', #2428, .T. ) ;
#2696 = PRODUCT_DEFINITION_SHAPE ( 'NONE', 'NONE',  #13150 ) ;
#2697 = CARTESIAN_POINT ( 'NONE',  ( -244.1419029264688447, -8.215433989563221573, 8.746719778172643345 ) ) ;
#2698 = CARTESIAN_POINT ( 'NONE',  ( -0.000000000000000000, -2.772967769358684720, 0.000000000000000000 ) ) ;
#2699 = ITEM_DEFINED_TRANSFORMATION ( 'NONE', 'NONE', #3349,  #805 ) ;
#2700 = ORIENTED_EDGE ( 'NONE', *, *, #161, .F. ) ;
#2701 = CARTESIAN_POINT ( 'NONE',  ( -286.5445428119863891, -18.00000000000000000, -22.67813138875635204 ) ) ;
#2702 = VERTEX_POINT ( 'NONE', #1974 ) ;
#2703 = CARTESIAN_POINT ( 'NONE',  ( -248.8121438751099959, -10.11580272835092842, -5.977715408740924552 ) ) ;
#2704 = ORIENTED_EDGE ( 'NONE', *, *, #3333, .F. ) ;
#2705 = EDGE_CURVE ( 'NONE', #9399, #3954, #8181, .T. ) ;
#2706 = AXIS2_PLACEMENT_3D ( 'NONE', #8624, #9490, #5426 ) ;
#2707 = CARTESIAN_POINT ( 'NONE',  ( 196.8887528222392973, 20.55460285123310982, 172.6991790951400390 ) ) ;
#2708 = ADVANCED_FACE ( 'NONE', ( #11168 ), #9239, .F. ) ;
#2709 = DIRECTION ( 'NONE',  ( 0.000000000000000000, -1.000000000000000000, 0.000000000000000000 ) ) ;
#2710 = CARTESIAN_POINT ( 'NONE',  ( -159.3442861576696998, -11.79660968244695951, -192.8974817588416784 ) ) ;
#2711 = CARTESIAN_POINT ( 'NONE',  ( -241.2613930295258911, 5.271300103320590402, 10.78025408308435118 ) ) ;
#2712 = EDGE_CURVE ( 'NONE', #3319, #7354, #6106, .T. ) ;
#2713 = FACE_OUTER_BOUND ( 'NONE', #12815, .T. ) ;
#2714 = CARTESIAN_POINT ( 'NONE',  ( -14.31396777367044315, -138.4705547276867321, -39.32730324096143448 ) ) ;
#2715 = CARTESIAN_POINT ( 'NONE',  ( 229.9948767726982908, 3.146592572275391131, 1.549747132302859320 ) ) ;
#2716 = AXIS2_PLACEMENT_3D ( 'NONE', #10132, #9589, #1069 ) ;
#2717 = AXIS2_PLACEMENT_3D ( 'NONE', #12810, #7749, #7807 ) ;
#2718 = CARTESIAN_POINT ( 'NONE',  ( -249.7718704160319589, 11.53079703974196946, 2.260598010248053402 ) ) ;
#2719 = CARTESIAN_POINT ( 'NONE',  ( -242.2842939340737303, -6.604577240716344555, -10.01896504309209490 ) ) ;
#2720 = CARTESIAN_POINT ( 'NONE',  ( -229.7140399059962590, -3.545728899456203287, -11.46574107171501211 ) ) ;
#2721 = ORIENTED_EDGE ( 'NONE', *, *, #1750, .F. ) ;
#2722 = ORIENTED_EDGE ( 'NONE', *, *, #10125, .F. ) ;
#2723 = CARTESIAN_POINT ( 'NONE',  ( 197.8197553893920144, 19.00000000000000000, 64.27553482998850143 ) ) ;
#2724 = EDGE_CURVE ( 'NONE', #9134, #3138, #7688, .T. ) ;
#2725 = DIRECTION ( 'NONE',  ( 0.000000000000000000, 1.000000000000000000, 0.000000000000000000 ) ) ;
#2726 = PRODUCT_DEFINITION_SHAPE ( 'NONE', 'NONE',  #13078 ) ;
#2727 = CARTESIAN_POINT ( 'NONE',  ( -17.06760680800445229, 20.79694577634651509, -260.7745447061710138 ) ) ;
#2728 = CONICAL_SURFACE ( 'NONE', #1682, 249.2999999999999829, 0.7853981633974207455 ) ;
#2729 = CARTESIAN_POINT ( 'NONE',  ( 224.4939760857161843, 0.000000000000000000, 0.000000000000000000 ) ) ;
#2730 = CARTESIAN_POINT ( 'NONE',  ( 0.000000000000000000, 0.000000000000000000, 0.000000000000000000 ) ) ;
#2731 = DIRECTION ( 'NONE',  ( 0.000000000000000000, 0.000000000000000000, 1.000000000000000000 ) ) ;
#2732 = CARTESIAN_POINT ( 'NONE',  ( 224.4939760857161843, 0.000000000000000000, 0.000000000000000000 ) ) ;
#2733 = AXIS2_PLACEMENT_3D ( 'NONE', #11603, #1332, #6472 ) ;
#2734 = ORIENTED_EDGE ( 'NONE', *, *, #10750, .T. ) ;
#2735 = CIRCLE ( 'NONE', #4653, 249.7999999999999829 ) ;
#2736 = CARTESIAN_POINT ( 'NONE',  ( -238.7263736996250145, -0.4312313169119866840, 11.99417204546059246 ) ) ;
#2737 = ORIENTED_EDGE ( 'NONE', *, *, #6959, .T. ) ;
#2738 = ORIENTED_EDGE ( 'NONE', *, *, #5494, .F. ) ;
#2739 = CARTESIAN_POINT ( 'NONE',  ( 71.82423009839129691, 30.00000000000000000, 197.3354503650404865 ) ) ;
#2740 = EDGE_LOOP ( 'NONE', ( #1694, #5351, #12010, #499 ) ) ;
#2741 = CARTESIAN_POINT ( 'NONE',  ( 0.000000000000000000, 29.00000000000000000, -208.0000000000000000 ) ) ;
#2742 =( REPRESENTATION_RELATIONSHIP ('NONE','NONE', #12019, #182 ) REPRESENTATION_RELATIONSHIP_WITH_TRANSFORMATION ( #3945 )SHAPE_REPRESENTATION_RELATIONSHIP( ) );
#2743 = CARTESIAN_POINT ( 'NONE',  ( -130.5770120874175859, 20.08915143279216764, 226.1171533172259842 ) ) ;
#2744 = LINE ( 'NONE', #6834, #6280 ) ;
#2745 = DIRECTION ( 'NONE',  ( 0.000000000000000000, 1.000000000000000000, 0.000000000000000000 ) ) ;
#2746 = AXIS2_PLACEMENT_3D ( 'NONE', #717, #6781, #5909 ) ;
#2747 = ORIENTED_EDGE ( 'NONE', *, *, #624, .T. ) ;
#2748 = FACE_OUTER_BOUND ( 'NONE', #5287, .T. ) ;
#2749 = ORIENTED_EDGE ( 'NONE', *, *, #9962, .T. ) ;
#2750 = CARTESIAN_POINT ( 'NONE',  ( -239.1925639823984397, 1.468143814834786953, 11.65791906053731708 ) ) ;
#2751 = VERTEX_POINT ( 'NONE', #5233 ) ;
#2752 = EDGE_CURVE ( 'NONE', #3580, #1937, #6425, .T. ) ;
#2753 =( REPRESENTATION_RELATIONSHIP ('NONE','NONE', #12019, #5191 ) REPRESENTATION_RELATIONSHIP_WITH_TRANSFORMATION ( #10476 )SHAPE_REPRESENTATION_RELATIONSHIP( ) );
#2754 = EDGE_CURVE ( 'NONE', #11433, #779, #908, .T. ) ;
#2755 = FACE_OUTER_BOUND ( 'NONE', #11403, .T. ) ;
#2756 = AXIS2_PLACEMENT_3D ( 'NONE', #11063, #5119, #8062 ) ;
#2757 = CARTESIAN_POINT ( 'NONE',  ( 240.2635760546321819, 2.467011616145750708, 2.483268943481589996 ) ) ;
#2758 = CARTESIAN_POINT ( 'NONE',  ( 0.000000000000000000, 19.00000000000000000, -208.0000000000000000 ) ) ;
#2759 = CARTESIAN_POINT ( 'NONE',  ( -247.3797639061697851, 9.674571922615484709, 6.668012154210222420 ) ) ;
#2760 = DIRECTION ( 'NONE',  ( 0.000000000000000000, -1.000000000000000000, 0.000000000000000000 ) ) ;
#2761 = CARTESIAN_POINT ( 'NONE',  ( -260.5542428351132571, 20.08915143297737060, -8.526617657838357900 ) ) ;
#2762 = AXIS2_PLACEMENT_3D ( 'NONE', #9316, #186, #2379 ) ;
#2763 = CARTESIAN_POINT ( 'NONE',  ( -244.4430806032956127, -8.412306923258608293, 8.557769328622804039 ) ) ;
#2764 = CARTESIAN_POINT ( 'NONE',  ( -91.90986972409933742, 20.79694577634647246, -244.1900186690937460 ) ) ;
#2765 = ITEM_DEFINED_TRANSFORMATION ( 'NONE', 'NONE', #11458,  #805 ) ;
#2766 = ORIENTED_EDGE ( 'NONE', *, *, #8533, .F. ) ;
#2767 = PRODUCT_DEFINITION ( 'UNKNOWN', '', #1081, #5963 ) ;
#2768 = CARTESIAN_POINT ( 'NONE',  ( 235.4000000000000057, 4.447920636657316074, -2.686261716586451520 ) ) ;
#2770 = ORIENTED_EDGE ( 'NONE', *, *, #2059, .T. ) ;
#2769 = PRODUCT_DEFINITION_FORMATION_WITH_SPECIFIED_SOURCE ( 'ANY', '', #115, .NOT_KNOWN. ) ;
#2771 = ORIENTED_EDGE ( 'NONE', *, *, #8334, .F. ) ;
#2772 = CARTESIAN_POINT ( 'NONE',  ( -249.6681481789321708, -11.15796663577227932, -3.682817568939428909 ) ) ;
#2773 = EDGE_LOOP ( 'NONE', ( #7756, #11313, #9549, #6631 ) ) ;
#2774 = CARTESIAN_POINT ( 'NONE',  ( 234.8993005733554185, 20.55460285121469610, -115.8123742911327838 ) ) ;
#2775 = LINE ( 'NONE', #4785, #1261 ) ;
#2776 = CARTESIAN_POINT ( 'NONE',  ( -189.4681260268063170, -29.00000000000000000, -229.3645116836740101 ) ) ;
#2777 = DIRECTION ( 'NONE',  ( 0.4503334343941555740, 0.7071067811865490160, 0.5451603414287971017 ) ) ;
#2778 = CIRCLE ( 'NONE', #1732, 5.099999999999993427 ) ;
#2779 = CARTESIAN_POINT ( 'NONE',  ( 27.68945685411497593, -30.00000000000000000, -290.6841825403026291 ) ) ;
#2780 = CARTESIAN_POINT ( 'NONE',  ( -166.5596220099214690, 3.327561323230709966, -201.6321540179175713 ) ) ;
#2781 = SURFACE_SIDE_STYLE ('',( #9126 ) ) ;
#2782 = DIRECTION ( 'NONE',  ( -1.000000000000000000, 0.000000000000000000, -6.982962677686266711E-15 ) ) ;
#2783 = EDGE_CURVE ( 'NONE', #10052, #7690, #6636, .T. ) ;
#2784 = CARTESIAN_POINT ( 'NONE',  ( 229.9737082357617624, 0.4553564789625448861, -3.477861664728034263 ) ) ;
#2785 = AXIS2_PLACEMENT_3D ( 'NONE', #10039, #7242, #975 ) ;
#2786 = EDGE_CURVE ( 'NONE', #6733, #5475, #7059, .T. ) ;
#2787 = CARTESIAN_POINT ( 'NONE',  ( -249.6893775634945598, 11.21617121202809564, -3.501676137307497605 ) ) ;
#2788 = CARTESIAN_POINT ( 'NONE',  ( 130.5770120874479971, 20.08915143273683412, 226.1171533175384809 ) ) ;
#2789 = CARTESIAN_POINT ( 'NONE',  ( -229.9653387109620724, -11.31703423231781080, 4.007864545467224815 ) ) ;
#2790 = ORIENTED_EDGE ( 'NONE', *, *, #1933, .T. ) ;
#2791 = ORIENTED_EDGE ( 'NONE', *, *, #7366, .F. ) ;
#2792 = AXIS2_PLACEMENT_3D ( 'NONE', #12863, #8610, #11810 ) ;
#2793 = LINE ( 'NONE', #11137, #9264 ) ;
#2794 = DIRECTION ( 'NONE',  ( 0.000000000000000000, 0.000000000000000000, 1.000000000000000000 ) ) ;
#2795 = B_SPLINE_CURVE_WITH_KNOTS ( 'NONE', 3,
 ( #11105, #10232, #10041, #2894, #5031, #6976, #6178, #8247, #2963, #12305, #2170, #977, #3905, #12969, #9241, #116, #6639, #5162, #4170, #1038, #11231, #6247, #10299, #8043, #1178, #3968, #4102, #1976 ),
 .UNSPECIFIED., .F., .F.,
 ( 4, 2, 1, 2, 2, 2, 1, 1, 2, 2, 2, 1, 1, 1, 2, 2, 4 ),
 ( 0.5011901855632154845, 0.5635414123677892073, 0.5947170257700761242, 0.6103048324712180284, 0.6258926391723599325, 0.6882438659769362088, 0.7194194793792243470, 0.7350072860803684716, 0.7428011894309405339, 0.7505950927815124851, 0.8129463195861132974, 0.8441219329884137590, 0.8597097396895591048, 0.8675036430401318333, 0.8714005947154180864, 0.8752975463907042286, 1.000000000000000000 ),
 .UNSPECIFIED. ) ;
#2796 = CARTESIAN_POINT ( 'NONE',  ( -207.3438552936920019, 20.79694577614539597, 159.0697709845790087 ) ) ;
#2797 = PLANE ( 'NONE',  #8591 ) ;
#2798 = PRODUCT_DEFINITION_SHAPE ( 'NONE', 'NONE',  #13165 ) ;
#2799 = DIRECTION ( 'NONE',  ( 0.8191520442889966835, 0.000000000000000000, -0.5735764363510391650 ) ) ;
#2800 = FACE_OUTER_BOUND ( 'NONE', #1117, .T. ) ;
#2801 = AXIS2_PLACEMENT_3D ( 'NONE', #1359, #2354, #8431 ) ;
#2802 = CARTESIAN_POINT ( 'NONE',  ( 122.2593324768334071, 19.00000000000000000, -168.2755348299895104 ) ) ;
#2803 = EDGE_CURVE ( 'NONE', #5993, #5992, #6177, .T. ) ;
#2804 = VERTEX_POINT ( 'NONE', #5977 ) ;
#2805 = CIRCLE ( 'NONE', #8785, 6.500000000000005329 ) ;
#2806 = DIRECTION ( 'NONE',  ( 0.000000000000000000, 0.000000000000000000, 1.000000000000000000 ) ) ;
#2807 = ORIENTED_EDGE ( 'NONE', *, *, #8666, .F. ) ;
#2808 = ORIENTED_EDGE ( 'NONE', *, *, #7306, .F. ) ;
#2809 = EDGE_CURVE ( 'NONE', #8685, #10853, #5133, .T. ) ;
#2810 = DIRECTION ( 'NONE',  ( 0.5469441386039890496, 0.000000000000000000, -0.8371691043312220470 ) ) ;
#2811 = ORIENTED_EDGE ( 'NONE', *, *, #12656, .F. ) ;
#2812 = PRODUCT_DEFINITION_SHAPE ( 'NONE', 'NONE',  #13140 ) ;
#2813 = CARTESIAN_POINT ( 'NONE',  ( 197.8197553893920144, 30.00000000000000000, 64.27553482998850143 ) ) ;
#2814 = FACE_OUTER_BOUND ( 'NONE', #288, .T. ) ;
#2815 = LINE ( 'NONE', #3694, #9660 ) ;
#2816 = SHAPE_REPRESENTATION_RELATIONSHIP ( 'NONE' , 'NONE' ,  #8443, #11752 ) ;
#2817 = DIRECTION ( 'NONE',  ( -0.4503334343941563511, -0.7071067811865480168, -0.5451603414287977678 ) ) ;
#2818 = VERTEX_POINT ( 'NONE', #11305 ) ;
#2819 = CARTESIAN_POINT ( 'NONE',  ( -239.0854549270513871, -1.310333253960263455, 11.67674951774069392 ) ) ;
#2820 = CONICAL_SURFACE ( 'NONE', #8377, 6.500000000000005329, 0.7853981633974476129 ) ;
#2821 = AXIS2_PLACEMENT_3D ( 'NONE', #6321, #10238, #9312 ) ;
#2822 = ORIENTED_EDGE ( 'NONE', *, *, #10221, .F. ) ;
#2823 = CARTESIAN_POINT ( 'NONE',  ( -245.3311829406554807, 8.905423747920915289, -7.665289359137143599 ) ) ;
#2824 = ORIENTED_EDGE ( 'NONE', *, *, #9863, .F. ) ;
#2825 = VECTOR ( 'NONE', #3740, 1000.000000000000000 ) ;
#2826 = CARTESIAN_POINT ( 'NONE',  ( -197.8197553893909912, 18.00000000000000000, 64.27553482999130097 ) ) ;
#2827 = CARTESIAN_POINT ( 'NONE',  ( 239.7985776503625175, 1.848645179571945185, 2.971954070985139751 ) ) ;
#2828 = CARTESIAN_POINT ( 'NONE',  ( 229.9000000000000057, 4.447920636657316074, -2.686261716586451520 ) ) ;
#2829 = CARTESIAN_POINT ( 'NONE',  ( 122.2593324768334071, 19.00000000000000000, -168.2755348299895104 ) ) ;
#2830 = CONICAL_SURFACE ( 'NONE', #1794, 5.500000000000015099, 0.7853981633974461696 ) ;
#2831 = FACE_BOUND ( 'NONE', #12509, .T. ) ;
#2832 = CARTESIAN_POINT ( 'NONE',  ( -240.7937243743992326, -4.465328607175659492, 11.13898957083963381 ) ) ;
#2833 = CARTESIAN_POINT ( 'NONE',  ( -239.2621195177060827, 1.577673499042776539, -11.89604841323225948 ) ) ;
#2834 = CONTEXT_DEPENDENT_SHAPE_REPRESENTATION ( #4376, #11897 ) ;
#2835 = VERTEX_POINT ( 'NONE', #4232 ) ;
#2836 = CARTESIAN_POINT ( 'NONE',  ( 122.2593324768346008, 19.00000000000000000, 168.2755348299889988 ) ) ;
#2837 = ADVANCED_FACE ( 'NONE', ( #11103 ), #10246, .F. ) ;
#2838 = VERTEX_POINT ( 'NONE', #113 ) ;
#2839 = TOROIDAL_SURFACE ( 'NONE', #7968, 250.3823410207189966, 3.000000000000000000 ) ;
#2840 = ORIENTED_EDGE ( 'NONE', *, *, #7148, .T. ) ;
#2841 = CARTESIAN_POINT ( 'NONE',  ( -249.7048772686739255, -11.25744417650646234, -3.375279419700558670 ) ) ;
#2842 = VERTEX_POINT ( 'NONE', #2167 ) ;
#2843 = CARTESIAN_POINT ( 'NONE',  ( -247.9906035374705766, 20.55460285117394648, 84.20717312385856701 ) ) ;
#2844 = CARTESIAN_POINT ( 'NONE',  ( 0.000000000000000000, 3.327561323230709966, 0.000000000000000000 ) ) ;
#2845 = CARTESIAN_POINT ( 'NONE',  ( -0.000000000000000000, -29.00000000000000000, 0.000000000000000000 ) ) ;
#2846 = AXIS2_PLACEMENT_3D ( 'NONE', #4503, #2446, #8589 ) ;
#2847 = B_SPLINE_CURVE_WITH_KNOTS ( 'NONE', 3,
 ( #9460, #3441, #3511, #11595, #6526, #8653, #6659, #10580, #1450, #9577, #7583, #457, #11656, #2509, #10647, #1587, #5648, #4384, #259, #4317, #8398, #4906, #12044, #10842, #650, #10907, #10978, #11038, #9840, #3768, #3712, #8979, #1714, #6724, #721, #3638, #4771, #8847, #1912, #9975, #9700, #5780, #1784, #12908, #847, #9909 ),
 .UNSPECIFIED., .F., .F.,
 ( 4, 2, 2, 1, 2, 2, 2, 2, 2, 2, 2, 2, 2, 2, 2, 2, 2, 2, 2, 2, 1, 2, 2, 4 ),
 ( 0.03674184081479667241, 0.03903768231472214134, 0.04018560306468487581, 0.04133352381464761027, 0.04248144456461034474, 0.04362936531457307920, 0.04592520681449854814, 0.04707312756446127566, 0.04822104831442401013, 0.05051688981434948600, 0.05166481056431222046, 0.05281273131427495493, 0.05510857281420043774, 0.05740441431412590667, 0.05855233506408864808, 0.05970025581405138948, 0.06199609731397685841, 0.06429193881390234122, 0.06658778031382781015, 0.06773570106379055156, 0.06888362181375329296, 0.07003154256371602049, 0.07117946331367874802, 0.07347530481360423082 ),
 .UNSPECIFIED. ) ;
#2848 = SPHERICAL_SURFACE ( 'NONE', #11070, 9.900000000000000355 ) ;
#2849 = CARTESIAN_POINT ( 'NONE',  ( -240.0622992133938851, -2.599441824298837300, 11.45917237866061456 ) ) ;
#2850 = CONICAL_SURFACE ( 'NONE', #9211, 6.500000000000005329, 0.7853981633974518317 ) ;
#2851 = AXIS2_PLACEMENT_3D ( 'NONE', #5939, #12268, #1869 ) ;
#2852 = DIRECTION ( 'NONE',  ( -0.4775568914688788635, 0.5538822189107471816, -0.6820219226572475923 ) ) ;
#2853 = DIRECTION ( 'NONE',  ( 0.4503334343941555740, 0.7071067811865490160, 0.5451603414287971017 ) ) ;
#2854 = EDGE_CURVE ( 'NONE', #4077, #6569, #8756, .T. ) ;
#2855 =( REPRESENTATION_RELATIONSHIP ('NONE','NONE', #12019, #5191 ) REPRESENTATION_RELATIONSHIP_WITH_TRANSFORMATION ( #480 )SHAPE_REPRESENTATION_RELATIONSHIP( ) );
#2856 = CARTESIAN_POINT ( 'NONE',  ( -229.9875200610103434, -11.75842346339721800, 2.402998940429985630 ) ) ;
#2857 = VERTEX_POINT ( 'NONE', #9304 ) ;
#2858 = ORIENTED_EDGE ( 'NONE', *, *, #9265, .F. ) ;
#2859 = AXIS2_PLACEMENT_3D ( 'NONE', #12266, #11259, #2121 ) ;
#2860 = CARTESIAN_POINT ( 'NONE',  ( 0.000000000000000000, 30.00000000000000000, 214.5000000000000000 ) ) ;
#2861 = CARTESIAN_POINT ( 'NONE',  ( 197.8197553893920144, 30.00000000000000000, 64.27553482998850143 ) ) ;
#2862 = ADVANCED_FACE ( 'NONE', ( #6312 ), #7487, .F. ) ;
#2863 = EDGE_CURVE ( 'NONE', #7702, #9318, #10461, .T. ) ;
#2864 = CARTESIAN_POINT ( 'NONE',  ( 234.3927740981229988, 20.79694577626769103, 115.5625104417014057 ) ) ;
#2865 = CARTESIAN_POINT ( 'NONE',  ( 181.8257142206846311, -30.00000000000000000, 220.1128339014740618 ) ) ;
#2866 = DIRECTION ( 'NONE',  ( 0.4226182617407064912, 0.000000000000000000, -0.9063077870366467170 ) ) ;
#2867 = CARTESIAN_POINT ( 'NONE',  ( -245.0626974418777309, -8.766422715046710223, 7.824416521862886498 ) ) ;
#2868 = CIRCLE ( 'NONE', #12672, 2.250000000000000000 ) ;
#2869 = ITEM_DEFINED_TRANSFORMATION ( 'NONE', 'NONE', #5927,  #805 ) ;
#2870 = VERTEX_POINT ( 'NONE', #6442 ) ;
#2871 = DIRECTION ( 'NONE',  ( -0.7709731485165535192, 0.000000000000000000, 0.6368676505102708330 ) ) ;
#2872 = DIRECTION ( 'NONE',  ( -0.000000000000000000, -1.000000000000000000, 0.000000000000000000 ) ) ;
#2873 = EDGE_LOOP ( 'NONE', ( #5833, #8453, #10259, #95 ) ) ;
#2874 = ORIENTED_EDGE ( 'NONE', *, *, #2705, .T. ) ;
#2875 = PRODUCT_DEFINITION_CONTEXT ( 'detailed design', #2333, 'design' ) ;
#2876 = LINE ( 'NONE', #5832, #5518 ) ;
#2877 = EDGE_LOOP ( 'NONE', ( #7953, #1892, #6337, #567 ) ) ;
#2878 = EDGE_CURVE ( 'NONE', #12286, #2427, #8571, .T. ) ;
#2879 = AXIS2_PLACEMENT_3D ( 'NONE', #2931, #9018, #12281 ) ;
#2880 = CARTESIAN_POINT ( 'NONE',  ( 185.9653539490014111, -18.00000000000000000, 225.1241593668316625 ) ) ;
#2881 = EDGE_CURVE ( 'NONE', #11832, #3272, #12213, .T. ) ;
#2882 = CARTESIAN_POINT ( 'NONE',  ( 158.9353507248500250, 20.08915143321791419, 207.1687172302519855 ) ) ;
#2883 = CARTESIAN_POINT ( 'NONE',  ( -238.6985546673921021, -0.1083677397390090530, -11.99999998179152172 ) ) ;
#2884 = CARTESIAN_POINT ( 'NONE',  ( 149.7885815989021694, -30.00000000000000000, 240.7652044943575333 ) ) ;
#2885 = EDGE_CURVE ( 'NONE', #3138, #3016, #9619, .T. ) ;
#2886 = VERTEX_POINT ( 'NONE', #7372 ) ;
#2887 = DIRECTION ( 'NONE',  ( 0.000000000000000000, 0.000000000000000000, 1.000000000000000000 ) ) ;
#2888 = VERTEX_POINT ( 'NONE', #9498 ) ;
#2889 = CARTESIAN_POINT ( 'NONE',  ( -239.1331745411521013, 1.386667391244157832, 11.66814598104677181 ) ) ;
#2890 = EDGE_LOOP ( 'NONE', ( #10477, #5720, #8784, #9481 ) ) ;
#2891 = DIRECTION ( 'NONE',  ( 1.000000000000000000, 0.000000000000000000, 0.000000000000000000 ) ) ;
#2892 = EDGE_CURVE ( 'NONE', #3737, #12029, #11579, .T. ) ;
#2893 = CARTESIAN_POINT ( 'NONE',  ( 240.2344515802825242, 2.410164965994779696, 2.538069655595715624 ) ) ;
#2894 = CARTESIAN_POINT ( 'NONE',  ( 238.9937144808838241, 0.3120165756308810878, 3.486321029130972082 ) ) ;
#2895 = DIRECTION ( 'NONE',  ( -1.000000000000000000, 0.000000000000000000, 0.000000000000000000 ) ) ;
#2896 = CYLINDRICAL_SURFACE ( 'NONE', #10301, 5.500000000000005329 ) ;
#2897 = CARTESIAN_POINT ( 'NONE',  ( -245.5719560650741187, -9.027896078068753383, 7.905358857528972827 ) ) ;
#2898 = CARTESIAN_POINT ( 'NONE',  ( -238.7338796418129050, 0.4303581359859351418, -11.99273839260487406 ) ) ;
#2899 = UNCERTAINTY_MEASURE_WITH_UNIT (LENGTH_MEASURE( 1.000000000000000082E-05 ), #10895, 'distance_accuracy_value', 'NONE');
#2900 = ORIENTED_EDGE ( 'NONE', *, *, #4675, .F. ) ;
#2901 = DIRECTION ( 'NONE',  ( 0.4503334343941441387, 0.7071067811865670016, 0.5451603414287832239 ) ) ;
#2902 = EDGE_LOOP ( 'NONE', ( #1577, #1656, #5673, #12493 ) ) ;
#2903 = EDGE_LOOP ( 'NONE', ( #7717, #10571, #7957, #9497 ) ) ;
#2904 = CARTESIAN_POINT ( 'NONE',  ( -248.0831933713610056, -9.830508068705260172, -6.436117704883899115 ) ) ;
#2905 = ORIENTED_EDGE ( 'NONE', *, *, #7767, .F. ) ;
#2906 = CARTESIAN_POINT ( 'NONE',  ( -115.8123742913374770, 20.55460285152583921, -234.8993005728878529 ) ) ;
#2907 = CARTESIAN_POINT ( 'NONE',  ( -247.9713910025420489, 9.811523844255248150, -6.908981293660537482 ) ) ;
#2908 = FACE_OUTER_BOUND ( 'NONE', #284, .T. ) ;
#2909 = DIRECTION ( 'NONE',  ( 0.000000000000000000, 1.000000000000000000, 0.000000000000000000 ) ) ;
#2910 = AXIS2_PLACEMENT_3D ( 'NONE', #2316, #8465, #3373 ) ;
#2911 = CARTESIAN_POINT ( 'NONE',  ( -242.4509935387671078, 6.787150506580164055, 9.898021028034207802 ) ) ;
#2912 = FACE_OUTER_BOUND ( 'NONE', #12450, .T. ) ;
#2913 = CARTESIAN_POINT ( 'NONE',  ( 37.93010648591186396, -138.4705547276867321, -17.68709912901486092 ) ) ;
#2914 = CARTESIAN_POINT ( 'NONE',  ( -229.6996680450365318, -0.3834651091013355773, 11.74999999999999645 ) ) ;
#2915 = CONTEXT_DEPENDENT_SHAPE_REPRESENTATION ( #5593, #2916 ) ;
#2916 = PRODUCT_DEFINITION_SHAPE ( 'NONE', 'NONE',  #13137 ) ;
#2917 = AXIS2_PLACEMENT_3D ( 'NONE', #10219, #10419, #7232 ) ;
#2918 = CARTESIAN_POINT ( 'NONE',  ( 135.8846079354933352, -18.00000000000000000, -256.1940150085812888 ) ) ;
#2919 = VERTEX_POINT ( 'NONE', #438 ) ;
#2920 = ORIENTED_EDGE ( 'NONE', *, *, #2125, .F. ) ;
#2921 = DIRECTION ( 'NONE',  ( 0.000000000000000000, 0.7071067811865470176, 0.7071067811865480168 ) ) ;
#2922 = DIRECTION ( 'NONE',  ( 0.000000000000000000, 0.000000000000000000, -1.000000000000000000 ) ) ;
#2923 = EDGE_CURVE ( 'NONE', #11199, #354, #5298, .T. ) ;
#2924 = EDGE_CURVE ( 'NONE', #3236, #11029, #372, .T. ) ;
#2925 = CARTESIAN_POINT ( 'NONE',  ( 153.9282213272189495, -28.60000000000000142, 245.7765299597151341 ) ) ;
#2926 = B_SPLINE_CURVE_WITH_KNOTS ( 'NONE', 3,
 ( #12977, #9590, #475, #9977, #8607, #2465, #8980, #4522, #6479, #12666, #6542, #4832, #4457, #5782, #3839, #12790, #7981, #5466, #8848, #9527, #1786, #10536, #9841, #1408, #11674, #9911, #3528, #7596, #12909, #3770, #406, #7840, #8542, #2761, #12601, #5853, #3459, #7537, #8915, #11610, #10162, #10302, #4104, #2041, #1041, #3031, #179, #8115, #12174, #9308, #12246, #7174, #2172, #4237, #6250, #7046, #6427, #4172, #1110, #1180, #9106, #8251, #12109, #12307, #3162, #51 ),
 .UNSPECIFIED., .F., .F.,
 ( 4, 2, 2, 2, 2, 2, 2, 2, 2, 2, 2, 2, 2, 2, 2, 2, 2, 2, 2, 2, 2, 2, 2, 2, 2, 2, 2, 2, 2, 2, 2, 2, 4 ),
 ( 0.000000000000000000, 0.01562500000000000347, 0.03125000000000001388, 0.04687500000000002776, 0.06250000000000001388, 0.07812500000000000000, 0.09374999999999998612, 0.1093749999999999861, 0.1249999999999999722, 0.1406249999999999722, 0.1562499999999999722, 0.1718749999999999722, 0.1874999999999999722, 0.2031250000000000000, 0.2187500000000000000, 0.2343750000000000000, 0.2500000000000000000, 0.2656250000000000000, 0.2812500000000000000, 0.2968750000000000000, 0.3125000000000000000, 0.3281250000000000000, 0.3437500000000000000, 0.3593750000000000000, 0.3750000000000000000, 0.3906250000000000555, 0.4062500000000000555, 0.4218750000000000555, 0.4375000000000000555, 0.4531250000000000555, 0.4687500000000000555, 0.4843750000000000555, 0.5000000000000000000 ),
 .UNSPECIFIED. ) ;
#2927 = DIRECTION ( 'NONE',  ( -1.000000000000000000, 0.000000000000000000, 0.000000000000000000 ) ) ;
#2928 = AXIS2_PLACEMENT_3D ( 'NONE', #8878, #12941, #8287 ) ;
#2929 = DIRECTION ( 'NONE',  ( -0.4503334343941595708, -0.7071067811865430208, -0.5451603414288016536 ) ) ;
#2930 = DIRECTION ( 'NONE',  ( -0.8191520442889871356, 0.000000000000000000, -0.5735764363510527097 ) ) ;
#2931 = CARTESIAN_POINT ( 'NONE',  ( 27.68945685411497593, -29.00000000000000000, -290.6841825403026291 ) ) ;
#2932 = CONTEXT_DEPENDENT_SHAPE_REPRESENTATION ( #12399, #4913 ) ;
#2933 = ORIENTED_EDGE ( 'NONE', *, *, #8894, .T. ) ;
#2934 = EDGE_CURVE ( 'NONE', #4597, #5366, #2195, .T. ) ;
#2935 = DIRECTION ( 'NONE',  ( 8.659560562354913137E-17, -0.7071067811865489050, 0.7071067811865460184 ) ) ;
#2936 = CARTESIAN_POINT ( 'NONE',  ( -238.9765878214913073, -1.145734732244408693, 11.94560817762122618 ) ) ;
#2937 = EDGE_LOOP ( 'NONE', ( #11224, #5310, #8901, #79 ) ) ;
#2938 = AXIS2_PLACEMENT_3D ( 'NONE', #893, #11408, #12157 ) ;
#2939 = EDGE_LOOP ( 'NONE', ( #10376, #8742, #1889, #856 ) ) ;
#2940 = VECTOR ( 'NONE', #666, 999.9999999999998863 ) ;
#2941 = CARTESIAN_POINT ( 'NONE',  ( 0.000000000000000000, 0.000000000000000000, 0.000000000000000000 ) ) ;
#2942 = LINE ( 'NONE', #11153, #11685 ) ;
#2943 = APPLICATION_CONTEXT ( 'automotive_design' ) ;
#2944 = VECTOR ( 'NONE', #8501, 999.9999999999998863 ) ;
#2945 = CIRCLE ( 'NONE', #12967, 5.500000000000015099 ) ;
#2946 = CARTESIAN_POINT ( 'NONE',  ( -249.2136238158385027, 10.44210856395644882, 5.387711592781305292 ) ) ;
#2947 = CONICAL_SURFACE ( 'NONE', #10949, 270.0000000000000000, 0.7853981633974476129 ) ;
#2948 = CONICAL_SURFACE ( 'NONE', #10409, 5.500000000000005329, 0.7853981633974461696 ) ;
#2949 = CARTESIAN_POINT ( 'NONE',  ( 226.1171533175249806, 20.08915143274010262, -130.5770120874387885 ) ) ;
#2950 = DIRECTION ( 'NONE',  ( 0.000000000000000000, -1.000000000000000000, 0.000000000000000000 ) ) ;
#2951 = CARTESIAN_POINT ( 'NONE',  ( -245.6111173893534385, 9.040876189779853078, 7.505250421144309847 ) ) ;
#2952 = CONICAL_SURFACE ( 'NONE', #1265, 250.7000000000000171, 0.7853981633974476129 ) ;
#2953 = ORIENTED_EDGE ( 'NONE', *, *, #10291, .T. ) ;
#2954 = DIRECTION ( 'NONE',  ( 0.000000000000000000, 1.000000000000000000, 0.000000000000000000 ) ) ;
#2955 = EDGE_CURVE ( 'NONE', #11853, #3329, #4119, .T. ) ;
#2956 = ORIENTED_EDGE ( 'NONE', *, *, #607, .F. ) ;
#2957 = EDGE_CURVE ( 'NONE', #3502, #8550, #7502, .T. ) ;
#2958 = CARTESIAN_POINT ( 'NONE',  ( -239.3015192883510736, 1.606994359549798856, 11.63956803321399391 ) ) ;
#2959 = ORIENTED_EDGE ( 'NONE', *, *, #9709, .T. ) ;
#2960 = AXIS2_PLACEMENT_3D ( 'NONE', #9306, #6443, #9374 ) ;
#2961 = CARTESIAN_POINT ( 'NONE',  ( 159.3442861576696998, 0.000000000000000000, 192.8974817588416784 ) ) ;
#2962 = FACE_OUTER_BOUND ( 'NONE', #3431, .T. ) ;
#2963 = CARTESIAN_POINT ( 'NONE',  ( 239.0510843050448671, 0.6173067666911031814, 3.446156762514750671 ) ) ;
#2964 = CARTESIAN_POINT ( 'NONE',  ( 235.4000000000000057, 0.000000000000000000, 0.000000000000000000 ) ) ;
#2965 = AXIS2_PLACEMENT_3D ( 'NONE', #5574, #9633, #9384 ) ;
#2966 = DIRECTION ( 'NONE',  ( -0.000000000000000000, -1.000000000000000000, 0.000000000000000000 ) ) ;
#2967 = SURFACE_STYLE_USAGE ( .BOTH. , #12377 ) ;
#2968 = CARTESIAN_POINT ( 'NONE',  ( -115.4021059068215180, 20.79694577634647246, -234.0054343868620492 ) ) ;
#2969 = ORIENTED_EDGE ( 'NONE', *, *, #7066, .T. ) ;
#2970 = CARTESIAN_POINT ( 'NONE',  ( -238.7110077732466777, -0.01032322003152743271, -11.74999631638433861 ) ) ;
#2971 = AXIS2_PLACEMENT_3D ( 'NONE', #11469, #7659, #7536 ) ;
#2972 = VERTEX_POINT ( 'NONE', #1372 ) ;
#2973 = ADVANCED_FACE ( 'NONE', ( #7434 ), #10630, .T. ) ;
#2974 = CARTESIAN_POINT ( 'NONE',  ( -243.4562500151471056, -7.708554438499255035, -9.196640587784429499 ) ) ;
#2975 = AXIS2_PLACEMENT_3D ( 'NONE', #10251, #8866, #11932 ) ;
#2976 = CARTESIAN_POINT ( 'NONE',  ( -249.5826926913502177, -10.95569487808942810, 4.257357224404557883 ) ) ;
#2977 = ORIENTED_EDGE ( 'NONE', *, *, #4837, .T. ) ;
#2978 = CARTESIAN_POINT ( 'NONE',  ( -252.4341100429099924, 20.79694577648418985, -67.61424743040240060 ) ) ;
#2979 = DIRECTION ( 'NONE',  ( -0.6368676505102707219, 0.000000000000000000, -0.7709731485165535192 ) ) ;
#2980 = DIRECTION ( 'NONE',  ( 0.000000000000000000, 0.000000000000000000, 1.000000000000000000 ) ) ;
#2981 = TOROIDAL_SURFACE ( 'NONE', #9379, 261.5294117647060261, 2.000000000000000000 ) ;
#2982 = CARTESIAN_POINT ( 'NONE',  ( -244.3371393051882876, -8.336835367652042805, -8.280174501370149542 ) ) ;
#2983 = CARTESIAN_POINT ( 'NONE',  ( -247.3711767300066811, 9.676486748390463077, 7.096931842783562594 ) ) ;
#2984 = AXIS2_PLACEMENT_3D ( 'NONE', #6415, #12535, #10474 ) ;
#2985 = CARTESIAN_POINT ( 'NONE',  ( 41.21542755584201956, -138.4705547276867321, -7.267391899529674681 ) ) ;
#2986 = DIRECTION ( 'NONE',  ( 0.000000000000000000, 0.000000000000000000, -1.000000000000000000 ) ) ;
#2987 = ITEM_DEFINED_TRANSFORMATION ( 'NONE', 'NONE', #866,  #805 ) ;
#2988 = FACE_OUTER_BOUND ( 'NONE', #2564, .T. ) ;
#2989 = ORIENTED_EDGE ( 'NONE', *, *, #8399, .T. ) ;
#2990 = EDGE_LOOP ( 'NONE', ( #6155, #5771, #7768, #1493 ) ) ;
#2991 = EDGE_CURVE ( 'NONE', #4661, #4062, #8892, .T. ) ;
#2992 = CARTESIAN_POINT ( 'NONE',  ( 235.0999999999999943, 0.000000000000000000, 0.000000000000000000 ) ) ;
#2993 = FACE_OUTER_BOUND ( 'NONE', #3241, .T. ) ;
#2994 = CARTESIAN_POINT ( 'NONE',  ( 238.9743710159888224, -9.335707311080796797E-14, -3.499999942258349428 ) ) ;
#2995 = CARTESIAN_POINT ( 'NONE',  ( -239.5361044668159991, -1.848645179572815156, 11.60366368868215758 ) ) ;
#2996 = AXIS2_PLACEMENT_3D ( 'NONE', #8904, #4902, #12905 ) ;
#2997 = CARTESIAN_POINT ( 'NONE',  ( -182.4625818711933221, -30.00000000000000000, -220.8838070499919013 ) ) ;
#2998 = DIRECTION ( 'NONE',  ( 0.7660444431189860071, 0.000000000000000000, -0.6427876096865301481 ) ) ;
#2999 = CARTESIAN_POINT ( 'NONE',  ( -244.2081860497233379, -8.251870589963452574, 8.364754208130431579 ) ) ;
#3000 = CONTEXT_DEPENDENT_SHAPE_REPRESENTATION ( #7974, #8780 ) ;
#3001 = AXIS2_PLACEMENT_3D ( 'NONE', #4618, #4425, #10570 ) ;
#3002 = APPLICATION_CONTEXT ( 'automotive_design' ) ;
#3003 = ORIENTED_EDGE ( 'NONE', *, *, #6858, .F. ) ;
#3004 = EDGE_CURVE ( 'NONE', #1017, #12496, #4323, .T. ) ;
#3005 = EDGE_CURVE ( 'NONE', #10483, #11299, #4486, .T. ) ;
#3006 = CARTESIAN_POINT ( 'NONE',  ( -238.8209209931138446, -0.7687232751576088541, 11.97535954172162853 ) ) ;
#3007 = ORIENTED_EDGE ( 'NONE', *, *, #11779, .T. ) ;
#3008 = ORIENTED_EDGE ( 'NONE', *, *, #371, .T. ) ;
#3009 = CARTESIAN_POINT ( 'NONE',  ( 0.000000000000000000, 1.848645179581460019, 0.000000000000000000 ) ) ;
#3010 = DIRECTION ( 'NONE',  ( 0.6368676505102707219, 0.000000000000000000, 0.7709731485165536302 ) ) ;
#3011 = CARTESIAN_POINT ( 'NONE',  ( -248.0831933713610056, 9.830508068705238856, 6.436117704883899115 ) ) ;
#3012 = CARTESIAN_POINT ( 'NONE',  ( -196.7513681801157759, 19.96883745974439961, 172.5787240288376836 ) ) ;
#3013 = FACE_OUTER_BOUND ( 'NONE', #7896, .T. ) ;
#3014 = DIRECTION ( 'NONE',  ( 1.000000000000000000, 0.000000000000000000, 0.000000000000000000 ) ) ;
#3015 = CARTESIAN_POINT ( 'NONE',  ( -245.4623802678685820, 8.970018888584359473, 7.589566415410549993 ) ) ;
#3016 = VERTEX_POINT ( 'NONE', #12693 ) ;
#3017 = LINE ( 'NONE', #5025, #10037 ) ;
#3018 = AXIS2_PLACEMENT_3D ( 'NONE', #10669, #10602, #7410 ) ;
#3019 = EDGE_CURVE ( 'NONE', #889, #4307, #84, .T. ) ;
#3020 = VERTEX_POINT ( 'NONE', #6510 ) ;
#3021 = CARTESIAN_POINT ( 'NONE',  ( -245.0626974371188567, 8.766422712495943514, -7.824416524692094477 ) ) ;
#3022 = ORIENTED_EDGE ( 'NONE', *, *, #1006, .F. ) ;
#3023 = AXIS2_PLACEMENT_3D ( 'NONE', #9428, #6497, #6361 ) ;
#3024 = AXIS2_PLACEMENT_3D ( 'NONE', #10367, #4173, #2102 ) ;
#3025 = CARTESIAN_POINT ( 'NONE',  ( 290.6841825403032544, -30.00000000000000000, 27.68945685411186730 ) ) ;
#3026 = CARTESIAN_POINT ( 'NONE',  ( 240.2035656452411558, 2.353769564626267297, 2.590352657692704508 ) ) ;
#3027 = CARTESIAN_POINT ( 'NONE',  ( 0.000000000000000000, 30.00000000000000000, -248.7999999999999829 ) ) ;
#3028 = EDGE_CURVE ( 'NONE', #8752, #8227, #11789, .T. ) ;
#3029 = DIRECTION ( 'NONE',  ( 0.000000000000000000, 1.000000000000000000, 0.000000000000000000 ) ) ;
#3030 = ADVANCED_FACE ( 'NONE', ( #312 ), #3043, .F. ) ;
#3031 = CARTESIAN_POINT ( 'NONE',  ( -211.9058003148605280, 20.08915143297737060, -151.8458048843646964 ) ) ;
#3032 = PRODUCT_DEFINITION_SHAPE ( 'NONE', 'NONE',  #13112 ) ;
#3033 = CARTESIAN_POINT ( 'NONE',  ( 71.82423009839129691, 30.00000000000000000, 197.3354503650404865 ) ) ;
#3034 = CARTESIAN_POINT ( 'NONE',  ( -196.1676464792609806, 20.79694577634646535, 172.0303573358519316 ) ) ;
#3035 = ORIENTED_EDGE ( 'NONE', *, *, #4231, .T. ) ;
#3036 = AXIS2_PLACEMENT_3D ( 'NONE', #10028, #4619, #10825 ) ;
#3037 = CARTESIAN_POINT ( 'NONE',  ( -239.2405902162603581, -1.531671746713636484, -11.64972311028024876 ) ) ;
#3038 = VERTEX_POINT ( 'NONE', #2365 ) ;
#3039 = CARTESIAN_POINT ( 'NONE',  ( -249.4806725022636442, 10.78221059153409733, -4.672140297476751414 ) ) ;
#3040 = DIRECTION ( 'NONE',  ( 0.000000000000000000, -1.000000000000000000, 0.000000000000000000 ) ) ;
#3041 = DIRECTION ( 'NONE',  ( -0.7709731485165536302, 0.000000000000000000, 0.6368676505102706109 ) ) ;
#3042 = ORIENTED_EDGE ( 'NONE', *, *, #10099, .T. ) ;
#3043 = CONICAL_SURFACE ( 'NONE', #4746, 6.499999999999999112, 0.7853981633974476129 ) ;
#3044 = AXIS2_PLACEMENT_3D ( 'NONE', #7699, #8516, #1506 ) ;
#3045 = CARTESIAN_POINT ( 'NONE',  ( -130.6873781523279945, 20.79694577633451402, 226.3083638767075172 ) ) ;
#3046 = DIRECTION ( 'NONE',  ( -0.000000000000000000, -1.000000000000000000, 0.000000000000000000 ) ) ;
#3047 = FACE_OUTER_BOUND ( 'NONE', #8727, .T. ) ;
#3048 = CARTESIAN_POINT ( 'NONE',  ( -247.3964713744789208, -9.678883351081529085, -6.661754107319017848 ) ) ;
#3049 = EDGE_CURVE ( 'NONE', #4180, #2640, #5693, .T. ) ;
#3050 = CARTESIAN_POINT ( 'NONE',  ( -243.4720072945636389, 7.721209754011274740, 9.186020676430386445 ) ) ;
#3051 = CARTESIAN_POINT ( 'NONE',  ( -24.18668477630638947, -29.00000000000000000, 294.9245348571438399 ) ) ;
#3052 = CARTESIAN_POINT ( 'NONE',  ( 39.32730324096147712, -138.4705547276867321, -14.31396777367031881 ) ) ;
#3053 = CARTESIAN_POINT ( 'NONE',  ( 225.1241593668336236, -30.00000000000000000, -185.9653539489990521 ) ) ;
#3054 = CONICAL_SURFACE ( 'NONE', #5189, 6.500000000000005329, 0.7853981633974518317 ) ;
#3055 = ADVANCED_FACE ( 'NONE', ( #4683 ), #1356, .F. ) ;
#3056 = ITEM_DEFINED_TRANSFORMATION ( 'NONE', 'NONE', #12997,  #805 ) ;
#3057 = AXIS2_PLACEMENT_3D ( 'NONE', #8472, #9403, #2396 ) ;
#3058 = FACE_OUTER_BOUND ( 'NONE', #8356, .T. ) ;
#3059 = ORIENTED_EDGE ( 'NONE', *, *, #7901, .F. ) ;
#3060 = EDGE_LOOP ( 'NONE', ( #1479, #7378, #3521, #2162, #1084, #11086, #8086, #10345 ) ) ;
#3061 = CARTESIAN_POINT ( 'NONE',  ( 34.10614053577565130, 20.08915143319461905, -258.8746690710824510 ) ) ;
#3062 = DIRECTION ( 'NONE',  ( 0.4503334343941626794, -0.7071067811865380248, 0.5451603414288055394 ) ) ;
#3063 = PRODUCT_DEFINITION_SHAPE ( 'NONE', 'NONE',  #13087 ) ;
#3064 = AXIS2_PLACEMENT_3D ( 'NONE', #4907, #849, #3908 ) ;
#3065 = DIRECTION ( 'NONE',  ( 0.000000000000000000, 1.000000000000000000, 0.000000000000000000 ) ) ;
#3066 = AXIS2_PLACEMENT_3D ( 'NONE', #2844, #4851, #10991 ) ;
#3067 = CARTESIAN_POINT ( 'NONE',  ( 130.6873781507030117, 20.79694577677803125, -226.3083638765525052 ) ) ;
#3068 = CARTESIAN_POINT ( 'NONE',  ( 0.000000000000000000, 20.00000000000000000, 0.000000000000000000 ) ) ;
#3069 = CARTESIAN_POINT ( 'NONE',  ( 0.000000000000000000, 0.000000000000000000, 0.000000000000000000 ) ) ;
#3070 = CARTESIAN_POINT ( 'NONE',  ( -243.5599937326495592, -7.782121668009089888, 8.802892756717024980 ) ) ;
#3071 = ITEM_DEFINED_TRANSFORMATION ( 'NONE', 'NONE', #1242,  #805 ) ;
#3072 = ORIENTED_EDGE ( 'NONE', *, *, #10308, .T. ) ;
#3073 = CARTESIAN_POINT ( 'NONE',  ( 7.960204194457795477E-16, 30.00000000000000000, -214.5000000000000000 ) ) ;
#3074 = VECTOR ( 'NONE', #656, 1000.000000000000000 ) ;
#3075 = DIRECTION ( 'NONE',  ( 0.000000000000000000, -1.000000000000000000, 0.000000000000000000 ) ) ;
#3076 = ORIENTED_EDGE ( 'NONE', *, *, #4669, .F. ) ;
#3077 = EDGE_LOOP ( 'NONE', ( #11633, #12821 ) ) ;
#3078 = CARTESIAN_POINT ( 'NONE',  ( 0.000000000000000000, 21.99999999999995381, 0.000000000000000000 ) ) ;
#3079 = EDGE_LOOP ( 'NONE', ( #5767, #532 ) ) ;
#3080 = EDGE_CURVE ( 'NONE', #2842, #11681, #10821, .T. ) ;
#3081 = CARTESIAN_POINT ( 'NONE',  ( -252.8031682270700458, 19.96883746027420869, -67.71318189758747508 ) ) ;
#3082 = VECTOR ( 'NONE', #8207, 1000.000000000000000 ) ;
#3083 = CARTESIAN_POINT ( 'NONE',  ( -239.9450917581429792, -2.156506209390995021, -11.80463811257499884 ) ) ;
#3084 = CARTESIAN_POINT ( 'NONE',  ( 0.000000000000000000, 0.000000000000000000, 0.000000000000000000 ) ) ;
#3085 = AXIS2_PLACEMENT_3D ( 'NONE', #308, #6240, #3346 ) ;
#3086 = CARTESIAN_POINT ( 'NONE',  ( -242.2664987710823823, 6.571392928988297299, 9.740637196669826636 ) ) ;
#3087 = ORIENTED_EDGE ( 'NONE', *, *, #92, .T. ) ;
#3088 = CARTESIAN_POINT ( 'NONE',  ( 260.3553053170167004, 20.79694577634646890, 17.06764083276451771 ) ) ;
#3089 = EDGE_LOOP ( 'NONE', ( #8659, #4063, #2807, #2159, #7868 ) ) ;
#3090 = DIRECTION ( 'NONE',  ( 0.000000000000000000, -0.01970892327970900221, -0.9998057603070482635 ) ) ;
#3091 = EDGE_LOOP ( 'NONE', ( #9421, #7564, #7783, #11776 ) ) ;
#3092 = AXIS2_PLACEMENT_3D ( 'NONE', #9737, #12812, #7751 ) ;
#3093 = B_SPLINE_CURVE_WITH_KNOTS ( 'NONE', 3,
 ( #5826, #10956, #9886, #4810, #7811, #3816, #10018, #5892, #11955, #6025, #9086, #1825, #820, #7956, #11085, #3642, #12025, #4884, #8956, #4007, #13018, #8090, #5960, #1952, #6955, #11014, #888, #4947, #8548, #3949, #2936, #5757, #7021, #12152, #3006, #8823, #10814, #9815, #11884, #2736, #1759, #12479 ),
 .UNSPECIFIED., .F., .F.,
 ( 4, 2, 2, 2, 2, 2, 2, 1, 1, 1, 2, 2, 2, 2, 1, 1, 2, 2, 2, 2, 1, 2, 2, 4 ),
 ( 0.000000000000000000, 0.06252861023063965851, 0.07034468650946289203, 0.07425272464887451573, 0.07816076278828612556, 0.09379291534592466839, 0.1094250679035632251, 0.1172411441823824341, 0.1211491823217919622, 0.1231032013914969692, 0.1240802109263322434, 0.1250572204611674898, 0.1875858306902031536, 0.2188501358047209855, 0.2344822883619798459, 0.2422983646406044467, 0.2462064027799215904, 0.2501144409192387341, 0.3126430511484086794, 0.3439073562629967884, 0.3595395088202907319, 0.3673555850989377869, 0.3751716613775847864, 0.5002288818359376110 ),
 .UNSPECIFIED. ) ;
#3094 = DIRECTION ( 'NONE',  ( -0.000000000000000000, -1.000000000000000000, 0.000000000000000000 ) ) ;
#3095 = DIRECTION ( 'NONE',  ( 0.000000000000000000, 0.000000000000000000, -1.000000000000000000 ) ) ;
#3096 = EDGE_CURVE ( 'NONE', #3954, #5655, #2678, .T. ) ;
#3097 = EDGE_CURVE ( 'NONE', #3301, #3428, #6470, .T. ) ;
#3098 = CYLINDRICAL_SURFACE ( 'NONE', #12182, 5.099999999999993427 ) ;
#3099 = DIRECTION ( 'NONE',  ( 0.6368676505102716101, 0.000000000000000000, 0.7709731485165527420 ) ) ;
#3100 = CARTESIAN_POINT ( 'NONE',  ( -0.000000000000000000, -19.00000000000000000, 0.000000000000000000 ) ) ;
#3101 = CARTESIAN_POINT ( 'NONE',  ( 0.000000000000000000, -22.00000000000000000, 0.000000000000000000 ) ) ;
#3102 = ORIENTED_EDGE ( 'NONE', *, *, #4505, .T. ) ;
#3103 = CARTESIAN_POINT ( 'NONE',  ( 0.000000000000000000, 18.00000000000000000, 0.000000000000000000 ) ) ;
#3104 = ORIENTED_EDGE ( 'NONE', *, *, #12408, .F. ) ;
#3105 = DIRECTION ( 'NONE',  ( 0.000000000000000000, 1.000000000000000000, 0.000000000000000000 ) ) ;
#3106 = CARTESIAN_POINT ( 'NONE',  ( -245.8375576770692987, -9.148519943277513278, -7.766315674714080686 ) ) ;
#3107 = EDGE_CURVE ( 'NONE', #9249, #10068, #12423, .T. ) ;
#3108 = CARTESIAN_POINT ( 'NONE',  ( -249.2798997179352796, -10.51457946798325160, 5.244637040187173582 ) ) ;
#3109 = EDGE_LOOP ( 'NONE', ( #2096, #6900, #1773, #4977 ) ) ;
#3110 = CARTESIAN_POINT ( 'NONE',  ( 207.3438552925264844, 20.79694577678052880, -159.0697709836649949 ) ) ;
#3111 = CARTESIAN_POINT ( 'NONE',  ( -245.5963909203066748, 9.039317601246798617, -7.892311131080197661 ) ) ;
#3112 = DIRECTION ( 'NONE',  ( -0.000000000000000000, -1.000000000000000000, 0.000000000000000000 ) ) ;
#3113 = CARTESIAN_POINT ( 'NONE',  ( -246.4924783784645399, -9.403937934938156218, -7.045599359059536937 ) ) ;
#3114 = CARTESIAN_POINT ( 'NONE',  ( 40.42519547187220041, -138.4705547276867321, 10.83189848055891424 ) ) ;
#3115 = CARTESIAN_POINT ( 'NONE',  ( -229.7074030909443252, -1.922301621807196881, 11.59804378764300736 ) ) ;
#3116 = AXIS2_PLACEMENT_3D ( 'NONE', #7356, #11489, #5613 ) ;
#3117 = EDGE_CURVE ( 'NONE', #1937, #8050, #12892, .T. ) ;
#3118 = EDGE_CURVE ( 'NONE', #2857, #10498, #6706, .T. ) ;
#3119 = CARTESIAN_POINT ( 'NONE',  ( -294.1869546181095529, -29.00000000000000000, -31.92980917095497517 ) ) ;
#3120 = ORIENTED_EDGE ( 'NONE', *, *, #1156, .F. ) ;
#3121 = VERTEX_POINT ( 'NONE', #12957 ) ;
#3122 = CARTESIAN_POINT ( 'NONE',  ( 115.4648407705614090, 20.08915143315789109, 234.1947771724234713 ) ) ;
#3123 = CARTESIAN_POINT ( 'NONE',  ( 229.9000000000000057, 0.4213317357727130452, -4.906371323945101004 ) ) ;
#3124 = DIRECTION ( 'NONE',  ( 0.000000000000000000, 1.000000000000000000, 0.000000000000000000 ) ) ;
#3125 = CARTESIAN_POINT ( 'NONE',  ( 171.9542656377731191, 19.00000000000000000, 208.1627500994694628 ) ) ;
#3126 = DIRECTION ( 'NONE',  ( -1.000000000000000000, 0.000000000000000000, 0.000000000000000000 ) ) ;
#3127 = DIRECTION ( 'NONE',  ( -0.7709731485165534082, 0.000000000000000000, 0.6368676505102708330 ) ) ;
#3128 = DIRECTION ( 'NONE',  ( 0.4226182617406879505, 0.000000000000000000, 0.9063077870366553768 ) ) ;
#3129 = CARTESIAN_POINT ( 'NONE',  ( -242.2606306403273209, -6.568547302997950865, 9.743049588217003176 ) ) ;
#3130 = ITEM_DEFINED_TRANSFORMATION ( 'NONE', 'NONE', #7416,  #805 ) ;
#3131 = CIRCLE ( 'NONE', #3984, 249.2999999999999829 ) ;
#3132 = EDGE_LOOP ( 'NONE', ( #9283, #13005, #12904, #9099 ) ) ;
#3133 =( REPRESENTATION_RELATIONSHIP ('NONE','NONE', #12019, #5191 ) REPRESENTATION_RELATIONSHIP_WITH_TRANSFORMATION ( #10586 )SHAPE_REPRESENTATION_RELATIONSHIP( ) );
#3134 = CARTESIAN_POINT ( 'NONE',  ( -221.6213872890270977, -30.00000000000000000, 190.2057062658400923 ) ) ;
#3135 = ADVANCED_FACE ( 'NONE', ( #5836 ), #7691, .T. ) ;
#3136 = FACE_OUTER_BOUND ( 'NONE', #11638, .T. ) ;
#3137 = EDGE_LOOP ( 'NONE', ( #10622, #369, #3399, #4261 ) ) ;
#3138 = VERTEX_POINT ( 'NONE', #11770 ) ;
#3139 = DIRECTION ( 'NONE',  ( 0.6368676505102707219, 0.000000000000000000, 0.7709731485165535192 ) ) ;
#3140 = DIRECTION ( 'NONE',  ( 0.000000000000000000, 0.000000000000000000, 1.000000000000000000 ) ) ;
#3141 = PRODUCT_DEFINITION_SHAPE ( 'NONE', 'NONE',  #13185 ) ;
#3142 = AXIS2_PLACEMENT_3D ( 'NONE', #101, #6362, #6234 ) ;
#3143 = CARTESIAN_POINT ( 'NONE',  ( -234.7354397751870749, 19.96883746042966123, 115.7315435905245522 ) ) ;
#3144 = CARTESIAN_POINT ( 'NONE',  ( -239.0453880742558113, -1.263976212796292353, -11.93324491903367068 ) ) ;
#3145 = CARTESIAN_POINT ( 'NONE',  ( 0.000000000000000000, 0.000000000000000000, 0.000000000000000000 ) ) ;
#3146 = CARTESIAN_POINT ( 'NONE',  ( -247.2571636853384405, 9.642662941262603482, 6.714255740641853265 ) ) ;
#3147 = EDGE_LOOP ( 'NONE', ( #11267, #7302, #267, #2721 ) ) ;
#3148 = VECTOR ( 'NONE', #9156, 1000.000000000000000 ) ;
#3149 = CIRCLE ( 'NONE', #12735, 3.153020646647511249 ) ;
#3150 = DIRECTION ( 'NONE',  ( 0.000000000000000000, 0.000000000000000000, 1.000000000000000000 ) ) ;
#3151 = CIRCLE ( 'NONE', #10610, 5.500000000000005329 ) ;
#3153 = ORIENTED_EDGE ( 'NONE', *, *, #11196, .F. ) ;
#3152 = AXIS2_PLACEMENT_3D ( 'NONE', #5887, #1880, #11077 ) ;
#3154 = DIRECTION ( 'NONE',  ( 0.9135454576426030870, -0.4066576386751317163, 0.008016341293427277012 ) ) ;
#3155 = VERTEX_POINT ( 'NONE', #8828 ) ;
#3156 = ORIENTED_EDGE ( 'NONE', *, *, #6606, .F. ) ;
#3157 = DIRECTION ( 'NONE',  ( -0.000000000000000000, -1.000000000000000000, 0.000000000000000000 ) ) ;
#3158 = DIRECTION ( 'NONE',  ( 0.000000000000000000, -1.000000000000000000, 0.000000000000000000 ) ) ;
#3159 = DIRECTION ( 'NONE',  ( -0.000000000000000000, -1.000000000000000000, 0.000000000000000000 ) ) ;
#3160 = DIRECTION ( 'NONE',  ( -0.4503334343941563511, -0.7071067811865480168, -0.5451603414287977678 ) ) ;
#3161 = AXIS2_PLACEMENT_3D ( 'NONE', #9925, #6865, #11927 ) ;
#3162 = CARTESIAN_POINT ( 'NONE',  ( -8.526617657837745057, 20.08915143297736705, -260.5542428351132571 ) ) ;
#3163 = DIRECTION ( 'NONE',  ( 0.000000000000000000, 1.000000000000000000, 0.000000000000000000 ) ) ;
#3164 = CIRCLE ( 'NONE', #6797, 6.500000000000000888 ) ;
#3165 = CONTEXT_DEPENDENT_SHAPE_REPRESENTATION ( #3180, #7744 ) ;
#3166 = ORIENTED_EDGE ( 'NONE', *, *, #7779, .F. ) ;
#3167 = DIRECTION ( 'NONE',  ( 0.000000000000000000, -0.7071067811865480168, -0.7071067811865470176 ) ) ;
#3168 = ORIENTED_EDGE ( 'NONE', *, *, #2783, .T. ) ;
#3169 = CARTESIAN_POINT ( 'NONE',  ( -239.5361044668155159, 1.848645179572584896, -11.60366368868220022 ) ) ;
#3170 = CARTESIAN_POINT ( 'NONE',  ( -243.2722961584167649, -7.557668641858518832, -9.321309795594205028 ) ) ;
#3171 = EDGE_CURVE ( 'NONE', #1172, #4030, #7103, .T. ) ;
#3172 = EDGE_CURVE ( 'NONE', #10034, #354, #1989, .T. ) ;
#3173 = VECTOR ( 'NONE', #12841, 1000.000000000000000 ) ;
#3174 = CARTESIAN_POINT ( 'NONE',  ( -248.9847817896189213, -10.23580904445972450, 5.770128483534315400 ) ) ;
#3175 = ORIENTED_EDGE ( 'NONE', *, *, #2036, .F. ) ;
#3176 = CARTESIAN_POINT ( 'NONE',  ( -84.02568524195829980, 20.79694577620390916, -247.4557548102065141 ) ) ;
#3177 = CARTESIAN_POINT ( 'NONE',  ( -243.5050917946776963, 7.747614400781131394, -9.163721889595233705 ) ) ;
#3178 = DIRECTION ( 'NONE',  ( -0.000000000000000000, -1.000000000000000000, 0.000000000000000000 ) ) ;
#3179 = CARTESIAN_POINT ( 'NONE',  ( -241.8928034536404255, -6.135811582726104163, -10.02290695296160017 ) ) ;
#3180 =( REPRESENTATION_RELATIONSHIP ('NONE','NONE', #12019, #182 ) REPRESENTATION_RELATIONSHIP_WITH_TRANSFORMATION ( #7178 )SHAPE_REPRESENTATION_RELATIONSHIP( ) );
#3181 = AXIS2_PLACEMENT_3D ( 'NONE', #4331, #7203, #6082 ) ;
#3182 = CARTESIAN_POINT ( 'NONE',  ( 239.4975972757000591, -1.524294659598023793, 3.150668454000119745 ) ) ;
#3183 = PRODUCT_DEFINITION_SHAPE ( 'NONE', 'NONE',  #13052 ) ;
#3184 = DIRECTION ( 'NONE',  ( -0.6427876096865327016, 0.000000000000000000, -0.7660444431189835646 ) ) ;
#3185 = CARTESIAN_POINT ( 'NONE',  ( -229.9813066729109039, 11.63677616891658140, -2.954026154813843785 ) ) ;
#3186 = DIRECTION ( 'NONE',  ( 0.000000000000000000, 0.9998057603070481525, -0.01970892327970899874 ) ) ;
#3187 = ORIENTED_EDGE ( 'NONE', *, *, #2923, .T. ) ;
#3188 = CARTESIAN_POINT ( 'NONE',  ( 67.55708173896789503, 20.08915143276009729, -252.2208631674930359 ) ) ;
#3189 = FACE_OUTER_BOUND ( 'NONE', #7380, .T. ) ;
#3190 =( REPRESENTATION_RELATIONSHIP ('NONE','NONE', #12019, #182 ) REPRESENTATION_RELATIONSHIP_WITH_TRANSFORMATION ( #5274 )SHAPE_REPRESENTATION_RELATIONSHIP( ) );
#3191 = CARTESIAN_POINT ( 'NONE',  ( 239.7985776503645354, -1.848645179573700004, -2.971954070984049956 ) ) ;
#3192 = AXIS2_PLACEMENT_3D ( 'NONE', #12795, #6806, #3659 ) ;
#3193 = CARTESIAN_POINT ( 'NONE',  ( -249.6387411364665923, 11.08439570754534387, 3.900217602256478067 ) ) ;
#3194 = LINE ( 'NONE', #2207, #2424 ) ;
#3195 = EDGE_CURVE ( 'NONE', #2427, #6421, #10073, .T. ) ;
#3196 = FACE_OUTER_BOUND ( 'NONE', #6862, .T. ) ;
#3197 = ADVANCED_FACE ( 'NONE', ( #10759 ), #4890, .T. ) ;
#3198 = CARTESIAN_POINT ( 'NONE',  ( 166.5596220099214406, 3.327561323230709966, 201.6321540179175997 ) ) ;
#3199 = DIRECTION ( 'NONE',  ( 0.9848077530122062440, 0.000000000000000000, 0.1736481776669404620 ) ) ;
#3200 = AXIS2_PLACEMENT_3D ( 'NONE', #5739, #4593, #9870 ) ;
#3201 = CARTESIAN_POINT ( 'NONE',  ( -210.0000000000000000, 30.00000000000000000, 0.000000000000000000 ) ) ;
#3202 = ORIENTED_EDGE ( 'NONE', *, *, #5128, .T. ) ;
#3203 = CARTESIAN_POINT ( 'NONE',  ( -225.1241593668336236, -19.00000000000000000, 185.9653539489990521 ) ) ;
#3204 = EDGE_CURVE ( 'NONE', #10691, #4229, #6359, .T. ) ;
#3205 = CARTESIAN_POINT ( 'NONE',  ( 229.9733680233431130, 4.286263893147487610E-16, -3.499999999999964917 ) ) ;
#3206 = ORIENTED_EDGE ( 'NONE', *, *, #7931, .T. ) ;
#3207 = ORIENTED_EDGE ( 'NONE', *, *, #6795, .F. ) ;
#3208 = DIRECTION ( 'NONE',  ( 0.000000000000000000, -1.000000000000000000, 0.000000000000000000 ) ) ;
#3209 = ORIENTED_EDGE ( 'NONE', *, *, #10916, .F. ) ;
#3210 = CARTESIAN_POINT ( 'NONE',  ( 261.1558126970361400, 19.96883746059272724, -17.09264059807959057 ) ) ;
#3211 = CONICAL_SURFACE ( 'NONE', #2577, 5.100000000000003197, 0.7853981633974461696 ) ;
#3212 = PRODUCT_DEFINITION_SHAPE ( 'NONE', 'NONE',  #13128 ) ;
#3213 = ADVANCED_FACE ( 'NONE', ( #4816 ), #9446, .T. ) ;
#3214 = CYLINDRICAL_SURFACE ( 'NONE', #4942, 249.7999999999999829 ) ;
#3215 = DIRECTION ( 'NONE',  ( 1.000000000000000000, 0.000000000000000000, 0.000000000000000000 ) ) ;
#3216 = CARTESIAN_POINT ( 'NONE',  ( -244.6792151888649016, 8.549823287007102479, 8.060814821815563747 ) ) ;
#3217 = ORIENTED_EDGE ( 'NONE', *, *, #11291, .F. ) ;
#3218 = CARTESIAN_POINT ( 'NONE',  ( 229.9733680233429993, 8.492964294626340574E-17, 3.499999999999964917 ) ) ;
#3219 = ADVANCED_FACE ( 'NONE', ( #10693 ), #6998, .F. ) ;
#3220 = ORIENTED_EDGE ( 'NONE', *, *, #12961, .F. ) ;
#3221 = LINE ( 'NONE', #4361, #6302 ) ;
#3222 = EDGE_LOOP ( 'NONE', ( #9599, #7422, #10241, #8859 ) ) ;
#3223 = EDGE_LOOP ( 'NONE', ( #4759, #11420, #5962, #11334 ) ) ;
#3224 = CONICAL_SURFACE ( 'NONE', #10682, 251.0000000000000000, 1.164698268477292631 ) ;
#3225 = CARTESIAN_POINT ( 'NONE',  ( 0.000000000000000000, -19.00000000000000000, 0.000000000000000000 ) ) ;
#3226 = FACE_OUTER_BOUND ( 'NONE', #9756, .T. ) ;
#3227 = LINE ( 'NONE', #12631, #11052 ) ;
#3228 = DIRECTION ( 'NONE',  ( 0.000000000000000000, 0.000000000000000000, 1.000000000000000000 ) ) ;
#3229 = CARTESIAN_POINT ( 'NONE',  ( -238.9324529062528484, 1.023324755385371265, -11.70535849071079859 ) ) ;
#3230 = DIRECTION ( 'NONE',  ( 0.000000000000000000, 0.000000000000000000, -1.000000000000000000 ) ) ;
#3231 = AXIS2_PLACEMENT_3D ( 'NONE', #8212, #1000, #11402 ) ;
#3232 = CONTEXT_DEPENDENT_SHAPE_REPRESENTATION ( #10761, #12852 ) ;
#3233 = EDGE_LOOP ( 'NONE', ( #5443, #4225, #11604, #11504 ) ) ;
#3234 = DIRECTION ( 'NONE',  ( 0.000000000000000000, 0.000000000000000000, 1.000000000000000000 ) ) ;
#3235 = AXIS2_PLACEMENT_3D ( 'NONE', #4353, #3277, #7360 ) ;
#3236 = VERTEX_POINT ( 'NONE', #9954 ) ;
#3237 = VECTOR ( 'NONE', #9824, 1000.000000000000114 ) ;
#3238 = CARTESIAN_POINT ( 'NONE',  ( 0.000000000000000000, 25.50000000000000000, 0.000000000000000000 ) ) ;
#3239 = CARTESIAN_POINT ( 'NONE',  ( -245.3462090897166661, -8.922924798440801553, -8.026147512420349628 ) ) ;
#3240 = CARTESIAN_POINT ( 'NONE',  ( -249.7849245721288867, -11.61140107739196559, 1.799432318634510919 ) ) ;
#3241 = EDGE_LOOP ( 'NONE', ( #307, #8037, #7759, #6714 ) ) ;
#3242 = CARTESIAN_POINT ( 'NONE',  ( -130.6873781513712061, 20.79694577639645203, -226.3083638771730079 ) ) ;
#3243 = CARTESIAN_POINT ( 'NONE',  ( -240.6982673021772712, 4.277714796599771496, -11.21297710698476102 ) ) ;
#3244 = DIRECTION ( 'NONE',  ( -0.000000000000000000, -0.5169713083949905030, -0.8560027256360646097 ) ) ;
#3245 = TOROIDAL_SURFACE ( 'NONE', #7303, 2.200000000000000178, 0.8000000000000000444 ) ;
#3246 = CARTESIAN_POINT ( 'NONE',  ( -245.8608051775114234, -9.153297364587587026, -7.368056644624257245 ) ) ;
#3247 = COLOUR_RGB ( '', 0.09019608, 0.27058824, 0.51372549) ;
#3248 = EDGE_CURVE ( 'NONE', #2094, #6789, #3790, .T. ) ;
#3249 = CARTESIAN_POINT ( 'NONE',  ( 239.5749691952057674, -1.619550703834554017, 3.102778355627506368 ) ) ;
#3250 = SHAPE_DEFINITION_REPRESENTATION ( #12566, #11671 ) ;
#3251 = CARTESIAN_POINT ( 'NONE',  ( 0.000000000000000000, -2.957522019940860139E-14, -241.5000000000000000 ) ) ;
#3252 = CIRCLE ( 'NONE', #1357, 5.099999999999993427 ) ;
#3253 = FACE_OUTER_BOUND ( 'NONE', #12448, .T. ) ;
#3254 = AXIS2_PLACEMENT_3D ( 'NONE', #1685, #9808, #7878 ) ;
#3255 = ORIENTED_EDGE ( 'NONE', *, *, #6938, .F. ) ;
#3256 = CARTESIAN_POINT ( 'NONE',  ( 258.8746690706134927, 20.08915143329815933, 34.10614053548034974 ) ) ;
#3257 = CARTESIAN_POINT ( 'NONE',  ( 197.8197553893915028, 19.00000000000000000, -64.27553482998990830 ) ) ;
#3258 = CARTESIAN_POINT ( 'NONE',  ( -249.2423535134873873, 10.47282816799440752, 5.327573254783502854 ) ) ;
#3259 = CARTESIAN_POINT ( 'NONE',  ( 189.4681260268079086, -30.00000000000000000, 229.3645116836727311 ) ) ;
#3260 = DIRECTION ( 'NONE',  ( 0.4503334343941562956, -0.7071067811865480168, 0.5451603414287978788 ) ) ;
#3261 = CARTESIAN_POINT ( 'NONE',  ( -210.0000000000000000, 30.00000000000000000, 6.500000000000000000 ) ) ;
#3262 = ADVANCED_FACE ( 'NONE', ( #13023 ), #2089, .T. ) ;
#3263 = CIRCLE ( 'NONE', #3698, 259.6078431372534396 ) ;
#3264 = CARTESIAN_POINT ( 'NONE',  ( 153.9282213272189495, -30.00000000000000000, 245.7765299597151341 ) ) ;
#3265 = DIRECTION ( 'NONE',  ( 0.9848077530122080203, 0.000000000000000000, 0.1736481776669307198 ) ) ;
#3266 = DIRECTION ( 'NONE',  ( -0.000000000000000000, -1.000000000000000000, 0.000000000000000000 ) ) ;
#3267 = CONTEXT_DEPENDENT_SHAPE_REPRESENTATION ( #2680, #803 ) ;
#3268 = EDGE_LOOP ( 'NONE', ( #4933, #11971, #5702, #8405, #11746, #4696 ) ) ;
#3269 = DIRECTION ( 'NONE',  ( 0.000000000000000000, 1.000000000000000000, 0.000000000000000000 ) ) ;
#3270 = CARTESIAN_POINT ( 'NONE',  ( 229.9849516113886807, -2.313877045632423357, 2.635927966202019412 ) ) ;
#3271 = ORIENTED_EDGE ( 'NONE', *, *, #12233, .T. ) ;
#3272 = VERTEX_POINT ( 'NONE', #633 ) ;
#3273 = EDGE_CURVE ( 'NONE', #6957, #6789, #8697, .T. ) ;
#3274 = CARTESIAN_POINT ( 'NONE',  ( -293.0608542803120145, -19.40000000000000213, 6.485521991431935973 ) ) ;
#3275 = DIRECTION ( 'NONE',  ( 0.7071067811865470176, -0.7069694329824861567, 0.01393631330096774257 ) ) ;
#3276 = CARTESIAN_POINT ( 'NONE',  ( 234.7354397751814759, 19.96883746015188876, -115.7315435904363312 ) ) ;
#3277 = DIRECTION ( 'NONE',  ( 0.000000000000000000, 1.000000000000000000, 0.000000000000000000 ) ) ;
#3278 = CARTESIAN_POINT ( 'NONE',  ( -220.9845196385168435, -18.00000000000000000, 190.9766794143566528 ) ) ;
#3279 = CIRCLE ( 'NONE', #11819, 6.500000000000005329 ) ;
#3280 = ORIENTED_EDGE ( 'NONE', *, *, #2624, .F. ) ;
#3281 = CARTESIAN_POINT ( 'NONE',  ( 17.06764083276447153, 20.79694577634646890, 260.3553053170167004 ) ) ;
#3282 = ORIENTED_EDGE ( 'NONE', *, *, #1270, .F. ) ;
#3283 = DIRECTION ( 'NONE',  ( 1.000000000000000000, 0.000000000000000000, 0.000000000000000000 ) ) ;
#3284 = ORIENTED_EDGE ( 'NONE', *, *, #1524, .F. ) ;
#3285 = EDGE_LOOP ( 'NONE', ( #3585, #7282, #7364, #8630 ) ) ;
#3286 = EDGE_CURVE ( 'NONE', #2618, #1953, #2204, .T. ) ;
#3287 = EDGE_CURVE ( 'NONE', #11992, #823, #5718, .T. ) ;
#3288 = STYLED_ITEM ( 'NONE', ( #4991 ), #5935 ) ;
#3289 = DIRECTION ( 'NONE',  ( 0.000000000000000000, 1.000000000000000000, 0.000000000000000000 ) ) ;
#3290 = FACE_BOUND ( 'NONE', #4731, .T. ) ;
#3291 = PRODUCT_DEFINITION_SHAPE ( 'NONE', 'NONE',  #13065 ) ;
#3292 = FACE_OUTER_BOUND ( 'NONE', #12831, .T. ) ;
#3293 = CARTESIAN_POINT ( 'NONE',  ( -229.6889200636375108, 1.000000000000000000, -11.95826074310140008 ) ) ;
#3294 = ADVANCED_FACE ( 'NONE', ( #7093 ), #7423, .F. ) ;
#3295 = DIRECTION ( 'NONE',  ( 0.000000000000000000, 0.000000000000000000, 1.000000000000000000 ) ) ;
#3296 = CARTESIAN_POINT ( 'NONE',  ( -246.2429388863588997, 9.313684383704458725, 7.566737218046005964 ) ) ;
#3297 = CONTEXT_DEPENDENT_SHAPE_REPRESENTATION ( #4797, #8304 ) ;
#3298 = ORIENTED_EDGE ( 'NONE', *, *, #7545, .F. ) ;
#3299 = DIRECTION ( 'NONE',  ( 0.000000000000000000, 1.000000000000000000, 0.000000000000000000 ) ) ;
#3300 = VECTOR ( 'NONE', #461, 1000.000000000000000 ) ;
#3301 = VERTEX_POINT ( 'NONE', #5335 ) ;
#3302 = TOROIDAL_SURFACE ( 'NONE', #3947, 241.5000000000000000, 2.500000000000000000 ) ;
#3303 = CARTESIAN_POINT ( 'NONE',  ( 122.2593324768346008, 18.00000000000000000, 168.2755348299889988 ) ) ;
#3304 = CARTESIAN_POINT ( 'NONE',  ( 227.3999999999999773, 0.000000000000000000, 0.000000000000000000 ) ) ;
#3305 = EDGE_CURVE ( 'NONE', #58, #11184, #6341, .T. ) ;
#3306 = CARTESIAN_POINT ( 'NONE',  ( 83.79436865282355029, 20.08915143297736705, 246.8597181602068815 ) ) ;
#3307 = ORIENTED_EDGE ( 'NONE', *, *, #12888, .T. ) ;
#3308 = B_SPLINE_CURVE_WITH_KNOTS ( 'NONE', 3,
 ( #8935, #5599, #5730, #3657, #6803, #6867, #9659, #9788, #3727, #7727, #12995, #669, #10731, #7793, #12722, #11863, #2711, #542, #8663, #1604, #10858, #740, #4790, #5665, #7861, #2653, #11929, #10928, #5373, #12503, #9445, #10062, #2911, #9064, #8384, #934, #317, #6381, #994, #6995, #4056, #3050, #242, #6004, #9997, #12059, #4300, #3986, #9124, #1, #7440, #11060, #10439, #10181, #5137, #12445, #8000, #4988, #6128, #4370, #3296, #3925, #9000, #5048, #865, #5932, #5306, #2298, #1059, #1309, #7377, #9377, #7065, #2983, #1931, #11440, #8450, #4926, #2056, #3354, #1997, #8061, #7134 ),
 .UNSPECIFIED., .F., .F.,
 ( 4, 2, 1, 1, 1, 2, 2, 2, 1, 1, 1, 1, 2, 2, 2, 2, 1, 1, 1, 1, 2, 2, 2, 2, 1, 1, 1, 2, 2, 2, 1, 1, 1, 1, 2, 2, 2, 2, 1, 1, 1, 2, 2, 2, 1, 1, 2, 2, 2, 1, 1, 2, 2, 4 ),
 ( 0.000000000000000000, 0.06250000000019761970, 0.09375000000029638791, 0.1093750000003448075, 0.1171875000003690104, 0.1210937500003811534, 0.1250000000003932965, 0.1875000000005736522, 0.2187500000006650791, 0.2343750000007107925, 0.2421875000007349399, 0.2460937500007456535, 0.2480468750007523426, 0.2500000000007590595, 0.3125000000009455770, 0.3437500000010404455, 0.3593750000010878520, 0.3671875000011132206, 0.3710937500011274870, 0.3730468750011329826, 0.3740234375011340928, 0.3750000000011352586, 0.4375000000010309531, 0.4687500000009787171, 0.4843750000009543477, 0.4921875000009404144, 0.4960937500009318657, 0.4980468750009276468, 0.5000000000009233725, 0.5625000000007391865, 0.5937500000006448175, 0.6093750000005976331, 0.6171875000005760947, 0.6210937500005654366, 0.6230468750005599965, 0.6250000000005546674, 0.6875000000004986012, 0.7187500000004706235, 0.7343750000004566347, 0.7421875000004468648, 0.7460937500004449774, 0.7480468750004409806, 0.7500000000004370948, 0.7812500000003682610, 0.7968750000003311795, 0.8046875000003151923, 0.8085937500003100853, 0.8125000000003048672, 0.8437500000002730038, 0.8593750000002597922, 0.8671875000002503553, 0.8710937500002429168, 0.8750000000002353673, 1.000000000000000000 ),
 .UNSPECIFIED. ) ;
#3309 = FACE_OUTER_BOUND ( 'NONE', #1497, .T. ) ;
#3310 = CARTESIAN_POINT ( 'NONE',  ( -243.2557941819830489, 7.548840537005648166, -9.332172160760025648 ) ) ;
#3311 = CARTESIAN_POINT ( 'NONE',  ( -239.6349225408002042, 1.943794467312871088, 11.84155609439077494 ) ) ;
#3312 = DIRECTION ( 'NONE',  ( 0.000000000000000000, 1.000000000000000000, 0.000000000000000000 ) ) ;
#3313 = PRESENTATION_STYLE_ASSIGNMENT (( #9461 ) ) ;
#3314 = APPLICATION_PROTOCOL_DEFINITION ( 'draft international standard', 'automotive_design', 1998, #8893 ) ;
#3315 = CARTESIAN_POINT ( 'NONE',  ( -229.7893046524160070, 6.871240432487316419, -9.845066738254859118 ) ) ;
#3316 = ITEM_DEFINED_TRANSFORMATION ( 'NONE', 'NONE', #5109,  #805 ) ;
#3317 = B_SPLINE_CURVE_WITH_KNOTS ( 'NONE', 3,
 ( #9284, #11283, #4208, #7220, #9531, #10408, #351, #6487, #3330, #5415, #1151, #155, #412, #4342, #1349, #11482, #2343, #8291 ),
 .UNSPECIFIED., .F., .F.,
 ( 4, 2, 2, 2, 2, 2, 2, 2, 4 ),
 ( 0.000000000000000000, 0.1249999999999946709, 0.1874999999999935607, 0.2499999999999924505, 0.4999999999999944489, 0.6249999999999954481, 0.6874999999999965583, 0.7499999999999976685, 1.000000000000000000 ),
 .UNSPECIFIED. ) ;
#3318 = DIRECTION ( 'NONE',  ( 0.000000000000000000, 1.000000000000000000, 0.000000000000000000 ) ) ;
#3319 = VERTEX_POINT ( 'NONE', #3955 ) ;
#3320 = CARTESIAN_POINT ( 'NONE',  ( 207.1687172321464914, 20.08915143279739013, 158.9353507257995091 ) ) ;
#3321 = DIRECTION ( 'NONE',  ( 0.7071067811865470176, 0.7069694329824861567, -0.01393631330096765583 ) ) ;
#3322 = DIRECTION ( 'NONE',  ( -0.000000000000000000, 1.000000000000000000, 0.000000000000000000 ) ) ;
#3323 = DIRECTION ( 'NONE',  ( 0.6368676505102716101, 0.000000000000000000, 0.7709731485165527420 ) ) ;
#3324 = DIRECTION ( 'NONE',  ( 0.6368676505102716101, 0.000000000000000000, 0.7709731485165527420 ) ) ;
#3325 = CARTESIAN_POINT ( 'NONE',  ( -246.3306884223085262, -9.347001913672279727, 7.525531261391552817 ) ) ;
#3326 = DIRECTION ( 'NONE',  ( 0.000000000000000000, 1.000000000000000000, 0.000000000000000000 ) ) ;
#3327 = CARTESIAN_POINT ( 'NONE',  ( -39.32730324096137764, -138.4705547276867321, 14.31396777367057815 ) ) ;
#3328 = CARTESIAN_POINT ( 'NONE',  ( 2.816687638038912194E-14, 0.000000000000000000, 230.0000000000000000 ) ) ;
#3329 = VERTEX_POINT ( 'NONE', #8345 ) ;
#3330 = CARTESIAN_POINT ( 'NONE',  ( 240.6324715325870045, -3.499918297958790170, -0.3875926898298525658 ) ) ;
#3331 = CARTESIAN_POINT ( 'NONE',  ( -229.8944816512308194, -9.773716331048332151, 6.972390473299147295 ) ) ;
#3332 = ORIENTED_EDGE ( 'NONE', *, *, #11735, .T. ) ;
#3333 = EDGE_CURVE ( 'NONE', #4800, #5845, #12200, .T. ) ;
#3334 = ORIENTED_EDGE ( 'NONE', *, *, #895, .F. ) ;
#3335 = EDGE_CURVE ( 'NONE', #3781, #11051, #11249, .T. ) ;
#3336 = LINE ( 'NONE', #7226, #12538 ) ;
#3337 = CARTESIAN_POINT ( 'NONE',  ( -190.1049936773165996, -30.00000000000000000, -230.1354848321905706 ) ) ;
#3338 = CARTESIAN_POINT ( 'NONE',  ( 247.8175805195787689, 19.96883746176681740, 84.14846197955617413 ) ) ;
#3339 = DIRECTION ( 'NONE',  ( 0.6368676505102716101, 0.000000000000000000, 0.7709731485165527420 ) ) ;
#3340 = DIRECTION ( 'NONE',  ( -0.7071067811865437980, 0.000000000000000000, -0.7071067811865512365 ) ) ;
#3341 = DIRECTION ( 'NONE',  ( 0.000000000000000000, -0.7071067811865489050, -0.7071067811865460184 ) ) ;
#3342 = CARTESIAN_POINT ( 'NONE',  ( -115.4021059068222570, 20.79694577634646535, 234.0054343868616797 ) ) ;
#3343 = ORIENTED_EDGE ( 'NONE', *, *, #8129, .F. ) ;
#3344 = CARTESIAN_POINT ( 'NONE',  ( 190.4297758776777982, 20.79694577634646180, 178.3611219674585584 ) ) ;
#3345 = VERTEX_POINT ( 'NONE', #1317 ) ;
#3346 = DIRECTION ( 'NONE',  ( 0.000000000000000000, 0.9998057603070481525, -0.01970892327970900221 ) ) ;
#3347 = ORIENTED_EDGE ( 'NONE', *, *, #6793, .F. ) ;
#3348 = ORIENTED_EDGE ( 'NONE', *, *, #8123, .T. ) ;
#3349 = AXIS2_PLACEMENT_3D ( 'NONE', #8169, #12230, #8366 ) ;
#3350 = DIRECTION ( 'NONE',  ( -0.6368676505102707219, 0.000000000000000000, -0.7709731485165535192 ) ) ;
#3351 = FACE_OUTER_BOUND ( 'NONE', #12237, .T. ) ;
#3352 = CARTESIAN_POINT ( 'NONE',  ( 239.5143764669230677, 1.545628038502534718, -3.140199926907355721 ) ) ;
#3353 = CARTESIAN_POINT ( 'NONE',  ( 235.4000000000000057, 4.550331206106116078, 2.508881407069060376 ) ) ;
#3354 = CARTESIAN_POINT ( 'NONE',  ( -247.9076433804861779, 9.798874666929192401, 6.926911304954392001 ) ) ;
#3355 = DIRECTION ( 'NONE',  ( 0.000000000000000000, -1.000000000000000000, 0.000000000000000000 ) ) ;
#3356 = EDGE_CURVE ( 'NONE', #368, #6293, #8518, .T. ) ;
#3357 = CIRCLE ( 'NONE', #12524, 246.0000000000000000 ) ;
#3358 = AXIS2_PLACEMENT_3D ( 'NONE', #10270, #4076, #9210 ) ;
#3359 = ADVANCED_FACE ( 'NONE', ( #4309 ), #10609, .F. ) ;
#3360 = ORIENTED_EDGE ( 'NONE', *, *, #655, .F. ) ;
#3361 = CARTESIAN_POINT ( 'NONE',  ( 2.400307726328812375E-14, 30.00000000000000000, -196.0000000000000000 ) ) ;
#3362 = ORIENTED_EDGE ( 'NONE', *, *, #11157, .T. ) ;
#3363 = DIRECTION ( 'NONE',  ( 0.000000000000000000, 1.000000000000000000, 0.000000000000000000 ) ) ;
#3364 = CARTESIAN_POINT ( 'NONE',  ( -285.6731895343928613, -18.00000000000000000, 15.42881051422396332 ) ) ;
#3365 = CARTESIAN_POINT ( 'NONE',  ( 107.5873595010540384, 20.08915143297736350, -237.4577367525705256 ) ) ;
#3366 = ORIENTED_EDGE ( 'NONE', *, *, #3546, .F. ) ;
#3367 = B_SPLINE_CURVE_WITH_KNOTS ( 'NONE', 3,
 ( #7814, #1762, #11890, #10889, #12954, #3819, #7885, #10959, #1354, #8297, #1220, #9289, #10346 ),
 .UNSPECIFIED., .F., .F.,
 ( 4, 2, 2, 1, 2, 2, 4 ),
 ( 0.000000000000000000, 0.2500000000000313083, 0.3750000000000306422, 0.4375000000000306422, 0.4687500000000305866, 0.5000000000000305311, 1.000000000000000000 ),
 .UNSPECIFIED. ) ;
#3368 = AXIS2_PLACEMENT_3D ( 'NONE', #10058, #11058, #9261 ) ;
#3369 = CYLINDRICAL_SURFACE ( 'NONE', #4037, 2.749999999999999556 ) ;
#3370 = CARTESIAN_POINT ( 'NONE',  ( -242.7490684365845084, 7.085544791023568045, -9.685620088677287853 ) ) ;
#3371 = DIRECTION ( 'NONE',  ( -1.000000000000000000, 0.000000000000000000, 0.000000000000000000 ) ) ;
#3372 = VECTOR ( 'NONE', #6154, 1000.000000000000000 ) ;
#3373 = DIRECTION ( 'NONE',  ( 0.000000000000000000, 0.000000000000000000, 1.000000000000000000 ) ) ;
#3374 = CIRCLE ( 'NONE', #411, 2.749999999999999556 ) ;
#3375 = AXIS2_PLACEMENT_3D ( 'NONE', #1203, #1133, #5192 ) ;
#3376 = EDGE_CURVE ( 'NONE', #1937, #3580, #12949, .T. ) ;
#3377 =( NAMED_UNIT ( * ) SI_UNIT ( $, .STERADIAN. ) SOLID_ANGLE_UNIT ( ) );
#3378 = APPLICATION_PROTOCOL_DEFINITION ( 'draft international standard', 'automotive_design', 1998, #7982 ) ;
#3379 = CARTESIAN_POINT ( 'NONE',  ( 240.6325187087303163, 3.500040777394010760, -0.1929172346387737214 ) ) ;
#3380 = ITEM_DEFINED_TRANSFORMATION ( 'NONE', 'NONE', #3834,  #805 ) ;
#3381 = VECTOR ( 'NONE', #5912, 1000.000000000000000 ) ;
#3382 = EDGE_CURVE ( 'NONE', #1401, #1635, #6386, .T. ) ;
#3383 = DIRECTION ( 'NONE',  ( -0.6368676505102706109, 0.000000000000000000, -0.7709731485165535192 ) ) ;
#3384 = VERTEX_POINT ( 'NONE', #11520 ) ;
#3385 = CARTESIAN_POINT ( 'NONE',  ( 130.8783844624215931, 19.96883746229290679, 226.6392846534563716 ) ) ;
#3386 = CARTESIAN_POINT ( 'NONE',  ( 0.000000000000000000, 0.000000000000000000, 0.000000000000000000 ) ) ;
#3387 = CARTESIAN_POINT ( 'NONE',  ( -164.6302876569050113, -3.165711975795909891E-14, -199.2965588915290596 ) ) ;
#3388 = DIRECTION ( 'NONE',  ( 0.6368676505102689456, 0.000000000000000000, 0.7709731485165549625 ) ) ;
#3389 = AXIS2_PLACEMENT_3D ( 'NONE', #4234, #3422, #9557 ) ;
#3390 = FACE_OUTER_BOUND ( 'NONE', #12955, .T. ) ;
#3391 = TOROIDAL_SURFACE ( 'NONE', #9184, 6.053020646647509828, 3.153020646647509917 ) ;
#3392 = CYLINDRICAL_SURFACE ( 'NONE', #11345, 246.0000000000000000 ) ;
#3393 = CARTESIAN_POINT ( 'NONE',  ( -37.93010648591173606, -138.4705547276867321, 17.68709912901511316 ) ) ;
#3394 = CARTESIAN_POINT ( 'NONE',  ( -247.1684828225455135, -9.630976094945838284, 6.736800401210575551 ) ) ;
#3395 = ITEM_DEFINED_TRANSFORMATION ( 'NONE', 'NONE', #11930,  #805 ) ;
#3396 = B_SPLINE_CURVE_WITH_KNOTS ( 'NONE', 3,
 ( #9593, #11866, #2784, #9719, #2656, #10735, #11812, #2534, #1607, #546, #4591, #3532, #478, #4792, #3597, #6612, #9867, #744, #6680, #11741, #5669, #2715, #7864, #8867, #4527, #6871, #11933, #6807, #12928, #5735, #1738, #8667 ),
 .UNSPECIFIED., .F., .F.,
 ( 4, 2, 2, 2, 2, 2, 2, 2, 2, 2, 2, 2, 2, 2, 2, 4 ),
 ( 0.01094275811428774454, 0.01162652601767144404, 0.01231029392105514354, 0.01299406182443884304, 0.01367782972782254428, 0.01436159763120624204, 0.01504536553458994327, 0.01572913343797364277, 0.01641290134135733880, 0.01709666924474104177, 0.01778043714812473780, 0.01846420505150844077, 0.01914797295489213680, 0.01983174085827583630, 0.02051550876165953580, 0.02188304456842693480 ),
 .UNSPECIFIED. ) ;
#3397 = PRODUCT_DEFINITION_SHAPE ( 'NONE', 'NONE',  #13072 ) ;
#3398 = CARTESIAN_POINT ( 'NONE',  ( -197.8197553893909912, 30.00000000000000000, 57.77553482999130807 ) ) ;
#3399 = ORIENTED_EDGE ( 'NONE', *, *, #5644, .T. ) ;
#3400 = ORIENTED_EDGE ( 'NONE', *, *, #9220, .F. ) ;
#3401 = AXIS2_PLACEMENT_3D ( 'NONE', #12131, #4127, #4992 ) ;
#3402 = DIRECTION ( 'NONE',  ( 0.000000000000000000, 1.000000000000000000, 0.000000000000000000 ) ) ;
#3403 = FACE_BOUND ( 'NONE', #4674, .T. ) ;
#3404 = TOROIDAL_SURFACE ( 'NONE', #7887, 250.7029414592220178, 3.000000000000000000 ) ;
#3405 = CARTESIAN_POINT ( 'NONE',  ( -159.4136521839998011, 20.55460285116278385, -207.7919029849606432 ) ) ;
#3406 = DIRECTION ( 'NONE',  ( 0.000000000000000000, 1.000000000000000000, 0.000000000000000000 ) ) ;
#3407 = DIRECTION ( 'NONE',  ( -0.8191520442889949072, 0.000000000000000000, 0.5735764363510416075 ) ) ;
#3408 = CARTESIAN_POINT ( 'NONE',  ( 197.8197553893920144, 19.00000000000000000, 64.27553482998850143 ) ) ;
#3409 = DIRECTION ( 'NONE',  ( -0.000000000000000000, -1.000000000000000000, 0.000000000000000000 ) ) ;
#3410 = ADVANCED_FACE ( 'NONE', ( #128 ), #8281, .F. ) ;
#3411 = LINE ( 'NONE', #8233, #3468 ) ;
#3412 = VERTEX_POINT ( 'NONE', #3169 ) ;
#3413 = CYLINDRICAL_SURFACE ( 'NONE', #5614, 195.0000000000000000 ) ;
#3414 = EDGE_LOOP ( 'NONE', ( #2629, #3343, #3814, #1579 ) ) ;
#3415 = CARTESIAN_POINT ( 'NONE',  ( 227.3999999999999773, -4.499125921381716076, 0.08869015475868961829 ) ) ;
#3416 = ORIENTED_EDGE ( 'NONE', *, *, #7386, .T. ) ;
#3417 = ORIENTED_EDGE ( 'NONE', *, *, #6841, .T. ) ;
#3418 = DIRECTION ( 'NONE',  ( 0.6368676505102707219, 0.000000000000000000, 0.7709731485165535192 ) ) ;
#3419 = CIRCLE ( 'NONE', #10036, 6.500000000000026645 ) ;
#3420 = DIRECTION ( 'NONE',  ( 0.000000000000000000, 0.000000000000000000, 1.000000000000000000 ) ) ;
#3421 = CIRCLE ( 'NONE', #9153, 12.00000000000000000 ) ;
#3422 = DIRECTION ( 'NONE',  ( 0.000000000000000000, 1.000000000000000000, 0.000000000000000000 ) ) ;
#3423 = CARTESIAN_POINT ( 'NONE',  ( 239.2930894857298370, 1.216635601427789704, -3.281912597133258114 ) ) ;
#3424 = CARTESIAN_POINT ( 'NONE',  ( -239.1925857173410748, 1.468173494105658117, -11.65791534653013350 ) ) ;
#3425 =( NAMED_UNIT ( * ) PLANE_ANGLE_UNIT ( ) SI_UNIT ( $, .RADIAN. ) );
#3426 = EDGE_CURVE ( 'NONE', #982, #4563, #5289, .T. ) ;
#3427 = AXIS2_PLACEMENT_3D ( 'NONE', #10158, #5161, #10101 ) ;
#3428 = VERTEX_POINT ( 'NONE', #7252 ) ;
#3429 = DIRECTION ( 'NONE',  ( -1.000000000000000000, 0.000000000000000000, 0.000000000000000000 ) ) ;
#3430 = ORIENTED_EDGE ( 'NONE', *, *, #5424, .T. ) ;
#3431 = EDGE_LOOP ( 'NONE', ( #7054, #12049, #3486, #5717 ) ) ;
#3432 =( REPRESENTATION_RELATIONSHIP ('NONE','NONE', #12019, #182 ) REPRESENTATION_RELATIONSHIP_WITH_TRANSFORMATION ( #12980 )SHAPE_REPRESENTATION_RELATIONSHIP( ) );
#3433 = CARTESIAN_POINT ( 'NONE',  ( 3.073828142905996055E-14, 22.00000000000000000, -250.7029414592220178 ) ) ;
#3434 = DIRECTION ( 'NONE',  ( 1.000000000000000000, 0.000000000000000000, 0.000000000000000000 ) ) ;
#3435 = CARTESIAN_POINT ( 'NONE',  ( 246.8597181602069384, 20.08915143297736350, 83.79436865282337976 ) ) ;
#3436 = EDGE_CURVE ( 'NONE', #12239, #7634, #8908, .T. ) ;
#3437 = DIRECTION ( 'NONE',  ( 0.000000000000000000, 0.9998057603070481525, -0.01970892327970899874 ) ) ;
#3438 = EDGE_CURVE ( 'NONE', #8275, #12029, #2181, .T. ) ;
#3439 = CARTESIAN_POINT ( 'NONE',  ( -244.1511139045946379, 8.221670796178244700, -8.740858669765747990 ) ) ;
#3440 = DIRECTION ( 'NONE',  ( 0.6368676505102707219, 0.000000000000000000, 0.7709731485165535192 ) ) ;
#3441 = CARTESIAN_POINT ( 'NONE',  ( -229.6996680450366455, 0.7667553648700247138, 11.75000000000000355 ) ) ;
#3442 = VECTOR ( 'NONE', #10505, 1000.000000000000000 ) ;
#3443 = CARTESIAN_POINT ( 'NONE',  ( 290.6841825403032544, -29.00000000000000000, 27.68945685411186730 ) ) ;
#3444 = SHAPE_DEFINITION_REPRESENTATION ( #2345, #5191 ) ;
#3445 = VECTOR ( 'NONE', #7711, 1000.000000000000000 ) ;
#3446 =( REPRESENTATION_RELATIONSHIP ('NONE','NONE', #12019, #5191 ) REPRESENTATION_RELATIONSHIP_WITH_TRANSFORMATION ( #11479 )SHAPE_REPRESENTATION_RELATIONSHIP( ) );
#3447 = CARTESIAN_POINT ( 'NONE',  ( -229.6921628766824313, 1.744838226299831874, 11.89597424155227401 ) ) ;
#3448 = ITEM_DEFINED_TRANSFORMATION ( 'NONE', 'NONE', #6403,  #805 ) ;
#3449 = CARTESIAN_POINT ( 'NONE',  ( 27.68945685411497593, -18.00000000000000000, -290.6841825403026291 ) ) ;
#3450 = ORIENTED_EDGE ( 'NONE', *, *, #5173, .F. ) ;
#3452 = EDGE_CURVE ( 'NONE', #3428, #12401, #3149, .T. ) ;
#3451 = CIRCLE ( 'NONE', #3023, 6.500000000000000888 ) ;
#3453 = CARTESIAN_POINT ( 'NONE',  ( -259.4723857429225404, 19.96883746178179209, 34.18476129330913693 ) ) ;
#3454 = EDGE_CURVE ( 'NONE', #5992, #9288, #4859, .T. ) ;
#3455 = DIRECTION ( 'NONE',  ( 0.000000000000000000, 0.000000000000000000, 1.000000000000000000 ) ) ;
#3456 = LINE ( 'NONE', #1336, #1787 ) ;
#3457 = AXIS2_PLACEMENT_3D ( 'NONE', #7765, #2745, #11024 ) ;
#3458 = FACE_OUTER_BOUND ( 'NONE', #3899, .T. ) ;
#3459 = CARTESIAN_POINT ( 'NONE',  ( -257.2112267038639288, 20.08915143297736705, -42.46883004693722796 ) ) ;
#3460 = EDGE_CURVE ( 'NONE', #8072, #5762, #12105, .T. ) ;
#3461 = PLANE ( 'NONE',  #4525 ) ;
#3462 = DIRECTION ( 'NONE',  ( -0.4162975160790987617, 0.5538822189107470706, 0.7210484489137187758 ) ) ;
#3463 = VECTOR ( 'NONE', #6018, 1000.000000000000000 ) ;
#3464 = DIRECTION ( 'NONE',  ( -0.6368676505102708330, 0.000000000000000000, -0.7709731485165536302 ) ) ;
#3465 = CIRCLE ( 'NONE', #10075, 5.099999999999993427 ) ;
#3466 = ITEM_DEFINED_TRANSFORMATION ( 'NONE', 'NONE', #6190,  #805 ) ;
#3467 = CONICAL_SURFACE ( 'NONE', #6473, 6.499999999999999112, 0.7853981633974476129 ) ;
#3468 = VECTOR ( 'NONE', #10214, 1000.000000000000114 ) ;
#3469 = CARTESIAN_POINT ( 'NONE',  ( -241.2864786002215851, -5.310083909452205653, -10.76118394184675964 ) ) ;
#3470 = AXIS2_PLACEMENT_3D ( 'NONE', #9875, #6690, #9672 ) ;
#3471 = CARTESIAN_POINT ( 'NONE',  ( -229.6921609078544577, -1.744386008313467240, 11.89601205791960936 ) ) ;
#3472 = ORIENTED_EDGE ( 'NONE', *, *, #6143, .F. ) ;
#3473 = ORIENTED_EDGE ( 'NONE', *, *, #3454, .F. ) ;
#3474 = DIRECTION ( 'NONE',  ( 0.000000000000000000, 0.000000000000000000, 1.000000000000000000 ) ) ;
#3475 = FACE_BOUND ( 'NONE', #5400, .T. ) ;
#3476 = AXIS2_PLACEMENT_3D ( 'NONE', #710, #7895, #3962 ) ;
#3477 = AXIS2_PLACEMENT_3D ( 'NONE', #7594, #4586, #6604 ) ;
#3478 = CARTESIAN_POINT ( 'NONE',  ( 247.8175805191053769, 19.96883746103348045, -84.14846197955421303 ) ) ;
#3479 = CARTESIAN_POINT ( 'NONE',  ( 197.8197553893920144, 30.00000000000000000, 57.77553482998850143 ) ) ;
#3480 = CARTESIAN_POINT ( 'NONE',  ( 0.000000000000000000, 0.000000000000000000, 0.000000000000000000 ) ) ;
#3481 = CARTESIAN_POINT ( 'NONE',  ( 2.828934106030385709E-14, -20.00000000000000000, 231.0000000000000000 ) ) ;
#3482 = FACE_OUTER_BOUND ( 'NONE', #7238, .T. ) ;
#3483 = VERTEX_POINT ( 'NONE', #11386 ) ;
#3484 = SPHERICAL_SURFACE ( 'NONE', #11590, 10.00000000000000000 ) ;
#3485 = AXIS2_PLACEMENT_3D ( 'NONE', #11967, #9830, #7826 ) ;
#3486 = ORIENTED_EDGE ( 'NONE', *, *, #9265, .T. ) ;
#3487 = CARTESIAN_POINT ( 'NONE',  ( 3.059167704270088292E-14, 21.50000000000000000, 249.7999999999999829 ) ) ;
#3488 = VERTEX_POINT ( 'NONE', #6323 ) ;
#3489 = EDGE_LOOP ( 'NONE', ( #2021, #11570, #4289, #4228 ) ) ;
#3490 = CIRCLE ( 'NONE', #10527, 5.499999999999986677 ) ;
#3491 = EDGE_CURVE ( 'NONE', #1921, #941, #12319, .T. ) ;
#3492 = DIRECTION ( 'NONE',  ( -0.000000000000000000, -1.000000000000000000, 0.000000000000000000 ) ) ;
#3493 = DIRECTION ( 'NONE',  ( -0.000000000000000000, -1.000000000000000000, 0.000000000000000000 ) ) ;
#3494 = DIRECTION ( 'NONE',  ( 0.000000000000000000, 1.000000000000000000, 0.000000000000000000 ) ) ;
#3495 = AXIS2_PLACEMENT_3D ( 'NONE', #8764, #7764, #3826 ) ;
#3496 = VECTOR ( 'NONE', #2853, 1000.000000000000000 ) ;
#3497 = CARTESIAN_POINT ( 'NONE',  ( -238.7452622531599502, 0.4192131502268354182, -11.74262611718073579 ) ) ;
#3498 = CARTESIAN_POINT ( 'NONE',  ( -285.6731895343928613, -30.00000000000000000, 15.42881051422395622 ) ) ;
#3499 = ITEM_DEFINED_TRANSFORMATION ( 'NONE', 'NONE', #7210,  #805 ) ;
#3500 = VERTEX_POINT ( 'NONE', #12451 ) ;
#3501 = CARTESIAN_POINT ( 'NONE',  ( -238.8442808645216076, -0.8022036787917719014, 11.72256788271878492 ) ) ;
#3502 = VERTEX_POINT ( 'NONE', #4434 ) ;
#3503 = DIRECTION ( 'NONE',  ( 0.000000000000000000, 0.000000000000000000, 1.000000000000000000 ) ) ;
#3504 = DIRECTION ( 'NONE',  ( 0.000000000000000000, -0.9998057603070481525, 0.01970892327970899874 ) ) ;
#3505 = AXIS2_PLACEMENT_3D ( 'NONE', #1875, #13007, #3869 ) ;
#3506 = EDGE_CURVE ( 'NONE', #11184, #8550, #822, .T. ) ;
#3507 = ADVANCED_FACE ( 'NONE', ( #1119 ), #9509, .F. ) ;
#3508 = LINE ( 'NONE', #5450, #4458 ) ;
#3509 = DIRECTION ( 'NONE',  ( -0.000000000000000000, -1.000000000000000000, 0.000000000000000000 ) ) ;
#3510 = CARTESIAN_POINT ( 'NONE',  ( -239.0270226278116752, 1.232440503845085411, 11.93654573081539816 ) ) ;
#3511 = CARTESIAN_POINT ( 'NONE',  ( -229.7035075530963582, 1.528882821208700893, 11.67566906642231395 ) ) ;
#3512 = CONICAL_SURFACE ( 'NONE', #7574, 5.500000000000005329, 0.7853981633974461696 ) ;
#3513 = CARTESIAN_POINT ( 'NONE',  ( -225.1241593668336236, -29.00000000000000000, 185.9653539489990521 ) ) ;
#3514 = APPLICATION_PROTOCOL_DEFINITION ( 'draft international standard', 'automotive_design', 1998, #3692 ) ;
#3515 = CONICAL_SURFACE ( 'NONE', #12040, 304.0000000000000000, 0.7853981633974207455 ) ;
#3516 = EDGE_CURVE ( 'NONE', #8008, #2888, #11318, .T. ) ;
#3517 = DIRECTION ( 'NONE',  ( -0.000000000000000000, -1.000000000000000000, 0.000000000000000000 ) ) ;
#3518 = CONTEXT_DEPENDENT_SHAPE_REPRESENTATION ( #2463, #1532 ) ;
#3519 = ORIENTED_EDGE ( 'NONE', *, *, #3708, .F. ) ;
#3520 = DIRECTION ( 'NONE',  ( 0.000000000000000000, -1.000000000000000000, 0.000000000000000000 ) ) ;
#3521 = ORIENTED_EDGE ( 'NONE', *, *, #6457, .T. ) ;
#3522 = AXIS2_PLACEMENT_3D ( 'NONE', #9517, #11794, #2639 ) ;
#3523 = CARTESIAN_POINT ( 'NONE',  ( -259.4723857429215741, 19.96883746091132394, -34.18476129331127567 ) ) ;
#3524 = LINE ( 'NONE', #11805, #8707 ) ;
#3525 = DIRECTION ( 'NONE',  ( 1.000000000000000000, 0.000000000000000000, 0.000000000000000000 ) ) ;
#3526 = LINE ( 'NONE', #5664, #9571 ) ;
#3527 = CONICAL_SURFACE ( 'NONE', #1836, 251.0000000000000000, 1.164698268477292631 ) ;
#3528 = CARTESIAN_POINT ( 'NONE',  ( -246.8597181602071657, 20.08915143297736705, 83.79436865282285396 ) ) ;
#3529 = CARTESIAN_POINT ( 'NONE',  ( -185.9653539489998195, -30.00000000000000000, -225.1241593668329699 ) ) ;
#3530 = DIRECTION ( 'NONE',  ( -0.5351817705578549855, 0.5538822189107471816, 0.6378047977532519397 ) ) ;
#3531 = EDGE_CURVE ( 'NONE', #6775, #10688, #9315, .T. ) ;
#3532 = CARTESIAN_POINT ( 'NONE',  ( 229.9933834991255139, 3.036879765700447820, -1.754926613119420331 ) ) ;
#3533 = EDGE_CURVE ( 'NONE', #3502, #58, #8063, .T. ) ;
#3534 = DIRECTION ( 'NONE',  ( -0.000000000000000000, 1.000000000000000000, 0.000000000000000000 ) ) ;
#3535 = DIRECTION ( 'NONE',  ( 0.000000000000000000, 1.000000000000000000, 0.000000000000000000 ) ) ;
#3536 = ORIENTED_EDGE ( 'NONE', *, *, #10139, .T. ) ;
#3537 = EDGE_LOOP ( 'NONE', ( #7971, #989, #8926, #6474 ) ) ;
#3538 = DIRECTION ( 'NONE',  ( 0.000000000000000000, 1.000000000000000000, 0.000000000000000000 ) ) ;
#3539 = CARTESIAN_POINT ( 'NONE',  ( 136.1890905123932498, -22.00000000000000000, -208.4551069784743333 ) ) ;
#3540 = CARTESIAN_POINT ( 'NONE',  ( 207.7919029844146053, 20.55460285114793351, 159.4136521835094413 ) ) ;
#3541 =( REPRESENTATION_RELATIONSHIP ('NONE','NONE', #12019, #5191 ) REPRESENTATION_RELATIONSHIP_WITH_TRANSFORMATION ( #10025 )SHAPE_REPRESENTATION_RELATIONSHIP( ) );
#3542 = CARTESIAN_POINT ( 'NONE',  ( 0.000000000000000000, 30.00000000000000000, 0.000000000000000000 ) ) ;
#3543 = CARTESIAN_POINT ( 'NONE',  ( 0.000000000000000000, 0.000000000000000000, 0.000000000000000000 ) ) ;
#3544 = DIRECTION ( 'NONE',  ( 0.000000000000000000, 0.000000000000000000, -1.000000000000000000 ) ) ;
#3545 = DIRECTION ( 'NONE',  ( 0.000000000000000000, 0.000000000000000000, 1.000000000000000000 ) ) ;
#3546 = EDGE_CURVE ( 'NONE', #6987, #10768, #9752, .T. ) ;
#3547 = ORIENTED_EDGE ( 'NONE', *, *, #10231, .T. ) ;
#3548 = CARTESIAN_POINT ( 'NONE',  ( 196.1676464792607248, 20.79694577634646890, -172.0303573358522726 ) ) ;
#3549 = VERTEX_POINT ( 'NONE', #3433 ) ;
#3550 = CIRCLE ( 'NONE', #2489, 6.500000000000005329 ) ;
#3551 = DIRECTION ( 'NONE',  ( 0.6368676505102707219, 0.000000000000000000, 0.7709731485165535192 ) ) ;
#3552 = ORIENTED_EDGE ( 'NONE', *, *, #9012, .F. ) ;
#3553 = VERTEX_POINT ( 'NONE', #452 ) ;
#3554 = CARTESIAN_POINT ( 'NONE',  ( -225.1241593668336236, -19.00000000000000000, 185.9653539489990521 ) ) ;
#3555 = VECTOR ( 'NONE', #9862, 1000.000000000000000 ) ;
#3556 = CARTESIAN_POINT ( 'NONE',  ( 239.0232640335058250, -0.4900023589501671384, -3.465599286982509408 ) ) ;
#3557 = DIRECTION ( 'NONE',  ( 1.224646799147353207E-16, -1.000000000000000000, 0.000000000000000000 ) ) ;
#3558 = DIRECTION ( 'NONE',  ( 0.6368676505102709440, 0.000000000000000000, 0.7709731485165532971 ) ) ;
#3559 = SHAPE_REPRESENTATION_RELATIONSHIP ( 'NONE' , 'NONE' ,  #12521, #6669 ) ;
#3560 =( LENGTH_UNIT ( ) NAMED_UNIT ( * ) SI_UNIT ( .MILLI., .METRE. ) );
#3561 = ITEM_DEFINED_TRANSFORMATION ( 'NONE', 'NONE', #12323,  #805 ) ;
#3562 = EDGE_LOOP ( 'NONE', ( #8213, #11924, #3430, #2359 ) ) ;
#3563 = LINE ( 'NONE', #5507, #1990 ) ;
#3565 = EDGE_LOOP ( 'NONE', ( #8340, #857, #6309, #886 ) ) ;
#3564 = AXIS2_PLACEMENT_3D ( 'NONE', #1025, #4155, #4022 ) ;
#3566 =( REPRESENTATION_RELATIONSHIP ('NONE','NONE', #12019, #5191 ) REPRESENTATION_RELATIONSHIP_WITH_TRANSFORMATION ( #6469 )SHAPE_REPRESENTATION_RELATIONSHIP( ) );
#3567 = CARTESIAN_POINT ( 'NONE',  ( -185.9653539489998195, -19.00000000000000000, -225.1241593668329699 ) ) ;
#3568 = DIRECTION ( 'NONE',  ( 0.000000000000000000, 0.000000000000000000, 1.000000000000000000 ) ) ;
#3569 = DIRECTION ( 'NONE',  ( 0.5469441386039890496, 0.000000000000000000, -0.8371691043312220470 ) ) ;
#3570 = DIRECTION ( 'NONE',  ( -0.000000000000000000, -1.000000000000000000, 0.000000000000000000 ) ) ;
#3571 = DIRECTION ( 'NONE',  ( -1.000000000000000000, -0.000000000000000000, -0.000000000000000000 ) ) ;
#3572 = CARTESIAN_POINT ( 'NONE',  ( 234.3487510399341716, 0.000000000000000000, 0.000000000000000000 ) ) ;
#3573 = AXIS2_PLACEMENT_3D ( 'NONE', #1360, #3340, #8679 ) ;
#3574 = CARTESIAN_POINT ( 'NONE',  ( -245.7661201684729804, -9.116795906119264714, 7.802929254751410859 ) ) ;
#3575 = CARTESIAN_POINT ( 'NONE',  ( 225.1241593668336236, -30.00000000000000000, -185.9653539489990521 ) ) ;
#3576 = ITEM_DEFINED_TRANSFORMATION ( 'NONE', 'NONE', #12090,  #805 ) ;
#3577 = EDGE_CURVE ( 'NONE', #9318, #7702, #10974, .T. ) ;
#3578 = CARTESIAN_POINT ( 'NONE',  ( -229.7805228887153817, 6.572088255991269001, 10.04733889956801107 ) ) ;
#3579 = EDGE_CURVE ( 'NONE', #12119, #1218, #12254, .T. ) ;
#3580 = VERTEX_POINT ( 'NONE', #9632 ) ;
#3581 = AXIS2_PLACEMENT_3D ( 'NONE', #10022, #10280, #4951 ) ;
#3582 = VECTOR ( 'NONE', #1272, 999.9999999999998863 ) ;
#3583 = CARTESIAN_POINT ( 'NONE',  ( 0.000000000000000000, 24.99999999999995737, -251.0000000000000000 ) ) ;
#3584 = AXIS2_PLACEMENT_3D ( 'NONE', #12690, #11762, #3551 ) ;
#3585 = ORIENTED_EDGE ( 'NONE', *, *, #12911, .F. ) ;
#3586 = CIRCLE ( 'NONE', #5079, 6.500000000000005329 ) ;
#3587 = CARTESIAN_POINT ( 'NONE',  ( 172.5787240287722284, 19.96883746003332405, -196.7513681799441656 ) ) ;
#3588 = CARTESIAN_POINT ( 'NONE',  ( -122.2593324768321992, 19.00000000000000000, 168.2755348299905052 ) ) ;
#3589 = DIRECTION ( 'NONE',  ( 0.000000000000000000, -1.000000000000000000, 0.000000000000000000 ) ) ;
#3590 = CONICAL_SURFACE ( 'NONE', #11481, 239.0000000000000000, 1.164698268477281307 ) ;
#3591 = PRODUCT_RELATED_PRODUCT_CATEGORY ( 'part', '', ( #8315 ) ) ;
#3592 = FACE_BOUND ( 'NONE', #9008, .T. ) ;
#3593 = CARTESIAN_POINT ( 'NONE',  ( -239.9440496357932204, -2.353898415756147777, 11.51208791644677731 ) ) ;
#3594 = AXIS2_PLACEMENT_3D ( 'NONE', #2099, #1107, #8381 ) ;
#3595 = DIRECTION ( 'NONE',  ( -1.000000000000000000, 0.000000000000000000, 0.000000000000000000 ) ) ;
#3596 = CARTESIAN_POINT ( 'NONE',  ( -41.21542755584196982, -138.4705547276867321, 7.267391899529953569 ) ) ;
#3597 = CARTESIAN_POINT ( 'NONE',  ( 229.9983154552353142, 3.387787197656995097, -0.9082533462923773060 ) ) ;
#3598 = COLOUR_RGB ( '', 0.31764706, 0.68627451, 0.89019608) ;
#3599 = CARTESIAN_POINT ( 'NONE',  ( 2.388061258337338860E-14, 19.00000000000000000, 195.0000000000000000 ) ) ;
#3600 = LINE ( 'NONE', #12730, #902 ) ;
#3601 = EDGE_LOOP ( 'NONE', ( #3153, #2260, #7322, #12971 ) ) ;
#3602 = ORIENTED_EDGE ( 'NONE', *, *, #8838, .T. ) ;
#3603 = AXIS2_PLACEMENT_3D ( 'NONE', #7503, #11574, #6512 ) ;
#3604 = DIRECTION ( 'NONE',  ( 0.6368676505102707219, 0.000000000000000000, 0.7709731485165535192 ) ) ;
#3605 = PLANE ( 'NONE',  #2202 ) ;
#3606 = EDGE_CURVE ( 'NONE', #1432, #8308, #5642, .T. ) ;
#3607 = EDGE_CURVE ( 'NONE', #9651, #11942, #6513, .T. ) ;
#3608 = CARTESIAN_POINT ( 'NONE',  ( 247.9906035370026984, 20.55460285091836070, -84.20717312441868785 ) ) ;
#3609 = DIRECTION ( 'NONE',  ( 1.000000000000000000, 0.000000000000000000, 0.000000000000000000 ) ) ;
#3610 = DIRECTION ( 'NONE',  ( -0.4226182617406942787, 0.000000000000000000, -0.9063077870366523792 ) ) ;
#3611 = FACE_OUTER_BOUND ( 'NONE', #3137, .T. ) ;
#3612 = CARTESIAN_POINT ( 'NONE',  ( -122.2593324768321992, 30.00000000000000000, 168.2755348299905052 ) ) ;
#3613 = AXIS2_PLACEMENT_3D ( 'NONE', #9860, #9786, #6740 ) ;
#3614 = ORIENTED_EDGE ( 'NONE', *, *, #11354, .T. ) ;
#3615 = CARTESIAN_POINT ( 'NONE',  ( 234.0054343868619355, 20.79694577634646890, -115.4021059068217738 ) ) ;
#3616 = DIRECTION ( 'NONE',  ( 0.7709731485165535192, -0.000000000000000000, -0.6368676505102707219 ) ) ;
#3617 = ORIENTED_EDGE ( 'NONE', *, *, #5384, .F. ) ;
#3618 = ORIENTED_EDGE ( 'NONE', *, *, #12187, .F. ) ;
#3619 = ORIENTED_EDGE ( 'NONE', *, *, #39, .F. ) ;
#3620 = DIRECTION ( 'NONE',  ( -0.4503334343941556295, 0.7071067811865489050, -0.5451603414287969906 ) ) ;
#3621 = EDGE_CURVE ( 'NONE', #9495, #5845, #3735, .T. ) ;
#3622 = LINE ( 'NONE', #8762, #7650 ) ;
#3623 = DIRECTION ( 'NONE',  ( 0.000000000000000000, 1.000000000000000000, 0.000000000000000000 ) ) ;
#3624 = AXIS2_PLACEMENT_3D ( 'NONE', #6466, #8595, #5585 ) ;
#3625 = LINE ( 'NONE', #1631, #9255 ) ;
#3626 =( NAMED_UNIT ( * ) PLANE_ANGLE_UNIT ( ) SI_UNIT ( $, .RADIAN. ) );
#3627 = EDGE_CURVE ( 'NONE', #8308, #6775, #4575, .T. ) ;
#3628 = ITEM_DEFINED_TRANSFORMATION ( 'NONE', 'NONE', #5065,  #805 ) ;
#3629 = ORIENTED_EDGE ( 'NONE', *, *, #10718, .F. ) ;
#3630 = DIRECTION ( 'NONE',  ( 0.000000000000000000, 0.7071067811865480168, 0.7071067811865470176 ) ) ;
#3631 = ORIENTED_EDGE ( 'NONE', *, *, #5666, .F. ) ;
#3632 = DIRECTION ( 'NONE',  ( -1.000000000000000000, 0.000000000000000000, 0.000000000000000000 ) ) ;
#3633 = ORIENTED_EDGE ( 'NONE', *, *, #6003, .T. ) ;
#3634 = VERTEX_POINT ( 'NONE', #8136 ) ;
#3635 = LINE ( 'NONE', #7977, #11536 ) ;
#3636 = DIRECTION ( 'NONE',  ( 0.000000000000000000, 0.7071067811865670016, 0.7071067811865280328 ) ) ;
#3637 = CARTESIAN_POINT ( 'NONE',  ( -130.7196491263534028, -23.50000000000000000, 200.0834159351620372 ) ) ;
#3638 = CARTESIAN_POINT ( 'NONE',  ( -229.8110182538512447, 7.181715867726937041, -9.331701923201524806 ) ) ;
#3639 = AXIS2_PLACEMENT_3D ( 'NONE', #7110, #11375, #12303 ) ;
#3640 = CARTESIAN_POINT ( 'NONE',  ( 197.8197553893920144, 30.00000000000000000, 69.77553482998851564 ) ) ;
#3641 = AXIS2_PLACEMENT_3D ( 'NONE', #1847, #11034, #5910 ) ;
#3642 = CARTESIAN_POINT ( 'NONE',  ( -239.4371284390123265, -1.766671737021507038, 11.86923926939766538 ) ) ;
#3643 = DIRECTION ( 'NONE',  ( -0.4503334343941556295, 0.7071067811865489050, -0.5451603414287969906 ) ) ;
#3644 = CARTESIAN_POINT ( 'NONE',  ( 131.7449682071765835, -30.00000000000000000, -261.2053404739389180 ) ) ;
#3645 = CONTEXT_DEPENDENT_SHAPE_REPRESENTATION ( #12437, #10469 ) ;
#3646 = EDGE_LOOP ( 'NONE', ( #2034, #9667 ) ) ;
#3647 = ORIENTED_EDGE ( 'NONE', *, *, #11244, .T. ) ;
#3648 = CARTESIAN_POINT ( 'NONE',  ( -249.2423535136895794, -10.47282816813556394, -5.327573254505493239 ) ) ;
#3649 = ORIENTED_EDGE ( 'NONE', *, *, #11496, .T. ) ;
#3650 = CARTESIAN_POINT ( 'NONE',  ( -234.7354397751870749, 19.96883746042966123, 115.7315435905245522 ) ) ;
#3651 = DIRECTION ( 'NONE',  ( 0.000000000000000000, 1.000000000000000000, 0.000000000000000000 ) ) ;
#3652 = DIRECTION ( 'NONE',  ( 0.6368676505102707219, 0.000000000000000000, 0.7709731485165536302 ) ) ;
#3653 = PRODUCT_DEFINITION_SHAPE ( 'NONE', 'NONE',  #13181 ) ;
#3654 = VECTOR ( 'NONE', #912, 1000.000000000000000 ) ;
#3655 = EDGE_CURVE ( 'NONE', #8497, #6601, #8355, .T. ) ;
#3656 = DIRECTION ( 'NONE',  ( 0.6368676505102707219, 0.000000000000000000, 0.7709731485165535192 ) ) ;
#3657 = CARTESIAN_POINT ( 'NONE',  ( -240.2229988807279426, 3.132498172464299735, 11.58475653428652308 ) ) ;
#3658 = DIRECTION ( 'NONE',  ( 0.000000000000000000, 1.000000000000000000, 0.000000000000000000 ) ) ;
#3659 = DIRECTION ( 'NONE',  ( -0.9961946980917448791, 0.000000000000000000, -0.08715574274766502150 ) ) ;
#3660 = CARTESIAN_POINT ( 'NONE',  ( -229.7576761218622892, -5.211361453271662114, -10.55923603912193798 ) ) ;
#3661 = CIRCLE ( 'NONE', #4649, 6.500000000000005329 ) ;
#3662 = ITEM_DEFINED_TRANSFORMATION ( 'NONE', 'NONE', #8532,  #805 ) ;
#3663 = PRODUCT_DEFINITION_SHAPE ( 'NONE', 'NONE',  #13147 ) ;
#3664 = CARTESIAN_POINT ( 'NONE',  ( -248.8927262318754856, 10.16869272944746427, -5.887412069865806785 ) ) ;
#3665 = LINE ( 'NONE', #3599, #12574 ) ;
#3666 = CARTESIAN_POINT ( 'NONE',  ( -229.9855622942915829, -11.72012966610593132, 2.583340135804222726 ) ) ;
#3667 = AXIS2_PLACEMENT_3D ( 'NONE', #4633, #1210, #12411 ) ;
#3668 = ORIENTED_EDGE ( 'NONE', *, *, #11615, .T. ) ;
#3669 = ORIENTED_EDGE ( 'NONE', *, *, #5588, .F. ) ;
#3670 = CARTESIAN_POINT ( 'NONE',  ( -159.9811538081799824, 20.00000000000000000, -193.6684549073582389 ) ) ;
#3671 = CARTESIAN_POINT ( 'NONE',  ( 153.9282213272189495, -19.40000000000000213, 245.7765299597151341 ) ) ;
#3672 = ADVANCED_FACE ( 'NONE', ( #1906 ), #3302, .F. ) ;
#3673 = AXIS2_PLACEMENT_3D ( 'NONE', #12216, #4001, #9141 ) ;
#3674 = CARTESIAN_POINT ( 'NONE',  ( -115.5625104413703923, 20.79694577664888300, 234.3927740973005029 ) ) ;
#3675 = DIRECTION ( 'NONE',  ( 0.000000000000000000, 0.000000000000000000, 1.000000000000000000 ) ) ;
#3676 = DIRECTION ( 'NONE',  ( -0.9063077870366467170, 0.000000000000000000, -0.4226182617407064912 ) ) ;
#3677 = STYLED_ITEM ( 'NONE', ( #7967 ), #10471 ) ;
#3678 = DIRECTION ( 'NONE',  ( 0.4503334343941555740, 0.7071067811865490160, 0.5451603414287971017 ) ) ;
#3679 = CARTESIAN_POINT ( 'NONE',  ( -197.8197553893909912, 19.00000000000000000, 64.27553482999130097 ) ) ;
#3680 = ORIENTED_EDGE ( 'NONE', *, *, #2691, .T. ) ;
#3681 = EDGE_CURVE ( 'NONE', #789, #12455, #11618, .T. ) ;
#3682 = CARTESIAN_POINT ( 'NONE',  ( -289.8128292627096130, -19.40000000000000213, 10.41748504886635907 ) ) ;
#3683 = ORIENTED_EDGE ( 'NONE', *, *, #1492, .T. ) ;
#3684 = ORIENTED_EDGE ( 'NONE', *, *, #6699, .F. ) ;
#3685 = AXIS2_PLACEMENT_3D ( 'NONE', #6831, #8891, #5896 ) ;
#3686 = VECTOR ( 'NONE', #246, 1000.000000000000114 ) ;
#3687 = CARTESIAN_POINT ( 'NONE',  ( 158.7026972336034021, 20.08915143297736705, 206.8203823583190797 ) ) ;
#3688 = VERTEX_POINT ( 'NONE', #9038 ) ;
#3689 = VECTOR ( 'NONE', #4475, 1000.000000000000114 ) ;
#3690 = DIRECTION ( 'NONE',  ( 1.000000000000000000, 0.000000000000000000, 0.000000000000000000 ) ) ;
#3691 = CARTESIAN_POINT ( 'NONE',  ( -240.0622992133934872, 2.599441824297004544, -11.45917237866102845 ) ) ;
#3692 = APPLICATION_CONTEXT ( 'automotive_design' ) ;
#3693 = DIRECTION ( 'NONE',  ( 0.000000000000000000, -0.7071067811865489050, -0.7071067811865460184 ) ) ;
#3694 = CARTESIAN_POINT ( 'NONE',  ( -171.9542656377731475, 0.000000000000000000, -208.1627500994694344 ) ) ;
#3695 = CARTESIAN_POINT ( 'NONE',  ( -249.7604317440018917, 11.15122115093721789, -4.588451767843126028 ) ) ;
#3696 = CARTESIAN_POINT ( 'NONE',  ( 0.000000000000000000, -19.00000000000000000, 249.7999999999999545 ) ) ;
#3697 = PRODUCT_DEFINITION_SHAPE ( 'NONE', 'NONE',  #7672 ) ;
#3698 = AXIS2_PLACEMENT_3D ( 'NONE', #4332, #5338, #4395 ) ;
#3699 = ORIENTED_EDGE ( 'NONE', *, *, #9789, .T. ) ;
#3700 = AXIS2_PLACEMENT_3D ( 'NONE', #5726, #12787, #12922 ) ;
#3701 = CARTESIAN_POINT ( 'NONE',  ( 0.000000000000000000, 0.000000000000000000, 0.000000000000000000 ) ) ;
#3702 = ADVANCED_FACE ( 'NONE', ( #4029 ), #8108, .T. ) ;
#3703 = ORIENTED_EDGE ( 'NONE', *, *, #6003, .F. ) ;
#3704 = ADVANCED_FACE ( 'NONE', ( #1300 ), #3515, .T. ) ;
#3705 = DIRECTION ( 'NONE',  ( -0.000000000000000000, -1.000000000000000000, 0.000000000000000000 ) ) ;
#3706 = VERTEX_POINT ( 'NONE', #1171 ) ;
#3707 = CIRCLE ( 'NONE', #2433, 3.000000000000000000 ) ;
#3708 = EDGE_CURVE ( 'NONE', #1614, #10046, #2163, .T. ) ;
#3709 = CARTESIAN_POINT ( 'NONE',  ( -189.4681260268063170, -19.00000000000000000, -229.3645116836740385 ) ) ;
#3710 = DIRECTION ( 'NONE',  ( -1.000000000000000000, 0.000000000000000000, 0.000000000000000000 ) ) ;
#3711 = CARTESIAN_POINT ( 'NONE',  ( -249.7969288063775366, -11.93744875558342855, 1.454679372137933191 ) ) ;
#3712 = CARTESIAN_POINT ( 'NONE',  ( -229.9422451730981436, 10.56339097491623491, -5.203035948314511216 ) ) ;
#3713 = CARTESIAN_POINT ( 'NONE',  ( -243.5376947841703270, -7.773445842367210368, 9.141748602850459093 ) ) ;
#3714 = DIRECTION ( 'NONE',  ( 0.000000000000000000, 0.000000000000000000, -1.000000000000000000 ) ) ;
#3715 = ORIENTED_EDGE ( 'NONE', *, *, #5156, .F. ) ;
#3716 = CARTESIAN_POINT ( 'NONE',  ( -229.8177839478270528, 7.761208678071466416, 9.154234884485560997 ) ) ;
#3717 = CIRCLE ( 'NONE', #10535, 2.500000000000002220 ) ;
#3718 = ORIENTED_EDGE ( 'NONE', *, *, #11421, .F. ) ;
#3719 = EDGE_CURVE ( 'NONE', #4133, #2702, #8637, .T. ) ;
#3720 = ORIENTED_EDGE ( 'NONE', *, *, #10099, .F. ) ;
#3721 = CARTESIAN_POINT ( 'NONE',  ( -248.7900388717992257, -10.10208648675346055, -6.000868149951671171 ) ) ;
#3722 = ORIENTED_EDGE ( 'NONE', *, *, #9547, .F. ) ;
#3723 = CARTESIAN_POINT ( 'NONE',  ( 247.9906035362907915, 20.55460285157398914, 84.20717312406510757 ) ) ;
#3724 = DIRECTION ( 'NONE',  ( 0.000000000000000000, 0.000000000000000000, 1.000000000000000000 ) ) ;
#3725 = CARTESIAN_POINT ( 'NONE',  ( -247.7878302976576776, -9.772649828929147020, -6.523883475188711145 ) ) ;
#3726 = CIRCLE ( 'NONE', #3505, 305.0000000000000000 ) ;
#3727 = CARTESIAN_POINT ( 'NONE',  ( -240.4767932493586784, 3.790394256715869492, 11.38565896274182521 ) ) ;
#3728 = FACE_OUTER_BOUND ( 'NONE', #12986, .T. ) ;
#3729 = CARTESIAN_POINT ( 'NONE',  ( -26.90145978217110212, -138.4705547276867321, -32.05991134143140187 ) ) ;
#3730 = CARTESIAN_POINT ( 'NONE',  ( -229.9848033347263652, -11.44892737729956345, -2.670968136663461667 ) ) ;
#3731 = CONTEXT_DEPENDENT_SHAPE_REPRESENTATION ( #10835, #2696 ) ;
#3732 = CARTESIAN_POINT ( 'NONE',  ( -249.7885090783126429, 11.63841215214888791, -1.617571259253988369 ) ) ;
#3733 = DIRECTION ( 'NONE',  ( 0.000000000000000000, 0.000000000000000000, 1.000000000000000000 ) ) ;
#3734 = CIRCLE ( 'NONE', #12891, 5.500000000000005329 ) ;
#3735 = B_SPLINE_CURVE_WITH_KNOTS ( 'NONE', 3,
 ( #2504, #7576, #7701, #10640, #12703, #8647, #11842, #2689, #5703, #11586, #5772, #1637, #4695, #9695, #10832, #1511, #9761, #2631, #7638, #6651, #643, #11649, #8772, #12836, #7771, #6779, #5573, #1706, #9832, #714, #517, #4763, #4566, #7515, #12578, #2441, #11716, #2567, #10708, #1580, #576, #4624, #8705, #7039, #3021, #6970, #3964, #2823, #1969, #1778, #1034, #7271, #9100, #904, #7972, #5975, #6912, #2033, #7829, #12903, #12099, #4899, #8036, #8971, #5906, #11903, #9901 ),
 .UNSPECIFIED., .F., .F.,
 ( 4, 2, 2, 1, 1, 1, 1, 2, 2, 2, 2, 2, 1, 1, 1, 1, 1, 2, 2, 2, 2, 2, 1, 1, 1, 2, 2, 2, 2, 1, 1, 1, 1, 2, 2, 2, 2, 1, 1, 1, 2, 2, 4 ),
 ( 0.000000000000000000, 0.1250000000007419343, 0.1875000000011130541, 0.2187500000012986556, 0.2343750000013898882, 0.2421875000014337698, 0.2460937500014541701, 0.2480468750014659107, 0.2500000000014776513, 0.3750000000022004065, 0.4375000000025618396, 0.4687500000027445268, 0.4843750000028378966, 0.4921875000028826386, 0.4960937500029050651, 0.4980468750029143910, 0.4990234375029189429, 0.4995117187529211078, 0.5000000000029232172, 0.5625000000027089442, 0.5937500000026018077, 0.6093750000025481839, 0.6171875000025213165, 0.6210937500025078828, 0.6230468750024996671, 0.6240234375024956703, 0.6250000000024915625, 0.6875000000021134205, 0.7187500000019271251, 0.7343750000018338664, 0.7421875000017872370, 0.7460937500017674751, 0.7480468750017541524, 0.7490234375017439383, 0.7500000000017337243, 0.8125000000012649881, 0.8437500000010332846, 0.8593750000009204859, 0.8671875000008643086, 0.8710937500008359979, 0.8730468750008220091, 0.8750000000008079093, 1.000000000000000000 ),
 .UNSPECIFIED. ) ;
#3736 = CARTESIAN_POINT ( 'NONE',  ( 0.000000000000000000, 30.00000000000000000, 208.0000000000000000 ) ) ;
#3737 = VERTEX_POINT ( 'NONE', #10357 ) ;
#3738 = VERTEX_POINT ( 'NONE', #109 ) ;
#3739 = CARTESIAN_POINT ( 'NONE',  ( -1.009475258464312158E-12, 20.08915143297736350, 260.5542428351129729 ) ) ;
#3740 = DIRECTION ( 'NONE',  ( 0.000000000000000000, -1.000000000000000000, 0.000000000000000000 ) ) ;
#3741 = CARTESIAN_POINT ( 'NONE',  ( -67.61424743045878927, 20.79694577628127661, -252.4341100433800023 ) ) ;
#3742 = DIRECTION ( 'NONE',  ( 0.000000000000000000, -0.7071067811865489050, -0.7071067811865460184 ) ) ;
#3743 = DIRECTION ( 'NONE',  ( 0.8660254037844432595, 0.000000000000000000, -0.4999999999999919509 ) ) ;
#3744 = CARTESIAN_POINT ( 'NONE',  ( -197.8197553893924976, 30.00000000000000000, -64.27553482998719403 ) ) ;
#3745 = CARTESIAN_POINT ( 'NONE',  ( 197.8197553893915028, 30.00000000000000000, -70.77553482998990830 ) ) ;
#3746 = ORIENTED_EDGE ( 'NONE', *, *, #5038, .F. ) ;
#3747 = EDGE_CURVE ( 'NONE', #3753, #678, #1395, .T. ) ;
#3748 = EDGE_CURVE ( 'NONE', #5508, #8628, #4227, .T. ) ;
#3749 = CARTESIAN_POINT ( 'NONE',  ( 0.000000000000000000, -2.772967769359314882, 240.3921568627447982 ) ) ;
#3750 = ORIENTED_EDGE ( 'NONE', *, *, #11172, .F. ) ;
#3751 = ORIENTED_EDGE ( 'NONE', *, *, #7660, .T. ) ;
#3752 = DIRECTION ( 'NONE',  ( 0.000000000000000000, -1.000000000000000000, 0.000000000000000000 ) ) ;
#3753 = VERTEX_POINT ( 'NONE', #6173 ) ;
#3754 = DIRECTION ( 'NONE',  ( 0.000000000000000000, 0.000000000000000000, 1.000000000000000000 ) ) ;
#3755 = DIRECTION ( 'NONE',  ( 0.6368676505102700558, 0.000000000000000000, 0.7709731485165541853 ) ) ;
#3756 = DIRECTION ( 'NONE',  ( 0.000000000000000000, 0.000000000000000000, -1.000000000000000000 ) ) ;
#3757 = CARTESIAN_POINT ( 'NONE',  ( -247.7878302962004113, 9.772649828613312550, 6.523883475601624404 ) ) ;
#3758 = AXIS2_PLACEMENT_3D ( 'NONE', #7873, #10874, #12938 ) ;
#3759 = EDGE_LOOP ( 'NONE', ( #4111, #11282 ) ) ;
#3760 = DIRECTION ( 'NONE',  ( -0.000000000000000000, -1.000000000000000000, 0.000000000000000000 ) ) ;
#3761 = EDGE_LOOP ( 'NONE', ( #10112, #3614, #10883, #8788 ) ) ;
#3762 = CARTESIAN_POINT ( 'NONE',  ( -239.2239471044186416, 1.510219371731709170, 11.65254212361304198 ) ) ;
#3763 = ORIENTED_EDGE ( 'NONE', *, *, #11496, .F. ) ;
#3764 = DIRECTION ( 'NONE',  ( 1.000000000000000000, 0.000000000000000000, 0.000000000000000000 ) ) ;
#3765 = FACE_OUTER_BOUND ( 'NONE', #4962, .T. ) ;
#3766 = CARTESIAN_POINT ( 'NONE',  ( 220.3999999999999773, 2.249562960690858038, -0.04434507737934524629 ) ) ;
#3767 = EDGE_CURVE ( 'NONE', #10938, #2233, #127, .T. ) ;
#3768 = CARTESIAN_POINT ( 'NONE',  ( -229.9631128808514973, 11.00533685364415248, -4.134445395687372127 ) ) ;
#3769 = EDGE_CURVE ( 'NONE', #8424, #379, #3221, .T. ) ;
#3770 = CARTESIAN_POINT ( 'NONE',  ( -257.2112267038639288, 20.08915143297736705, 42.46883004693641084 ) ) ;
#3771 = PRODUCT_DEFINITION_SHAPE ( 'NONE', 'NONE',  #13156 ) ;
#3772 = CARTESIAN_POINT ( 'NONE',  ( -242.6565957993711322, -6.994822106563381325, 9.751204008824640113 ) ) ;
#3773 = CARTESIAN_POINT ( 'NONE',  ( -67.53249125288850507, 20.79694577634646890, -252.0229195836992631 ) ) ;
#3774 = CONTEXT_DEPENDENT_SHAPE_REPRESENTATION ( #7535, #6291 ) ;
#3775 = ORIENTED_EDGE ( 'NONE', *, *, #7056, .F. ) ;
#3776 = LINE ( 'NONE', #12914, #12242 ) ;
#3777 = ITEM_DEFINED_TRANSFORMATION ( 'NONE', 'NONE', #12781,  #805 ) ;
#3778 = ORIENTED_EDGE ( 'NONE', *, *, #1708, .T. ) ;
#3779 = ORIENTED_EDGE ( 'NONE', *, *, #8425, .T. ) ;
#3780 = CARTESIAN_POINT ( 'NONE',  ( -249.6727234477500588, -11.17009475776062821, -3.645778574373556680 ) ) ;
#3781 = VERTEX_POINT ( 'NONE', #4163 ) ;
#3782 = CARTESIAN_POINT ( 'NONE',  ( -17.10461161402953323, 20.55460285106647689, -261.3381329044966606 ) ) ;
#3783 = FACE_OUTER_BOUND ( 'NONE', #3091, .T. ) ;
#3784 = CARTESIAN_POINT ( 'NONE',  ( -290.6841825403030839, -19.00000000000000000, -27.68945685411394919 ) ) ;
#3785 = DIRECTION ( 'NONE',  ( 0.000000000000000000, 0.000000000000000000, 1.000000000000000000 ) ) ;
#3786 = EDGE_CURVE ( 'NONE', #9988, #8945, #8433, .T. ) ;
#3787 = FACE_OUTER_BOUND ( 'NONE', #5863, .T. ) ;
#3788 = CARTESIAN_POINT ( 'NONE',  ( 149.7885815989021694, -18.00000000000000000, 240.7652044943575333 ) ) ;
#3789 = DIRECTION ( 'NONE',  ( -0.5735764363510498232, 0.000000000000000000, 0.8191520442889891340 ) ) ;
#3790 = CIRCLE ( 'NONE', #1888, 251.8333333333299606 ) ;
#3791 = CARTESIAN_POINT ( 'NONE',  ( 165.3358371128620377, -2.772967769358684720, 200.1506762031205255 ) ) ;
#3792 = AXIS2_PLACEMENT_3D ( 'NONE', #752, #4802, #11071 ) ;
#3793 = EDGE_CURVE ( 'NONE', #6648, #2275, #5221, .T. ) ;
#3794 = CIRCLE ( 'NONE', #11251, 4.000000000000000000 ) ;
#3795 = ITEM_DEFINED_TRANSFORMATION ( 'NONE', 'NONE', #4048,  #805 ) ;
#3796 = AXIS2_PLACEMENT_3D ( 'NONE', #10203, #950, #2998 ) ;
#3797 = AXIS2_PLACEMENT_3D ( 'NONE', #287, #5277, #8159 ) ;
#3798 = CARTESIAN_POINT ( 'NONE',  ( -249.7845350863069029, 11.60862138571708968, -1.817256861374815458 ) ) ;
#3799 = CARTESIAN_POINT ( 'NONE',  ( -242.6194444000231840, -6.961689675190617876, -9.776526358366776748 ) ) ;
#3800 = CARTESIAN_POINT ( 'NONE',  ( -229.9454081747827559, -10.90707088183632578, -5.058745115878076959 ) ) ;
#3801 = ORIENTED_EDGE ( 'NONE', *, *, #6936, .F. ) ;
#3802 = EDGE_LOOP ( 'NONE', ( #3618, #8370, #5090, #5144, #5344, #6956 ) ) ;
#3803 = DIRECTION ( 'NONE',  ( 0.000000000000000000, -1.000000000000000000, 0.000000000000000000 ) ) ;
#3804 = DIRECTION ( 'NONE',  ( 0.000000000000000000, 1.000000000000000000, 0.000000000000000000 ) ) ;
#3805 = PRODUCT ( 'Precision Steel Bearing Balls', 'Precision Steel Bearing Balls', '', ( #5521 ) ) ;
#3806 = VECTOR ( 'NONE', #6477, 1000.000000000000000 ) ;
#3807 = CARTESIAN_POINT ( 'NONE',  ( -252.4341100429099924, 20.79694577648418985, -67.61424743040240060 ) ) ;
#3808 = AXIS2_PLACEMENT_3D ( 'NONE', #1087, #11288, #10484 ) ;
#3809 = DIRECTION ( 'NONE',  ( -0.000000000000000000, -1.000000000000000000, 0.000000000000000000 ) ) ;
#3810 = DIRECTION ( 'NONE',  ( 0.5735764363510527097, 0.000000000000000000, -0.8191520442889871356 ) ) ;
#3811 = DIRECTION ( 'NONE',  ( 0.000000000000000000, 0.000000000000000000, 1.000000000000000000 ) ) ;
#3812 = DIRECTION ( 'NONE',  ( 0.000000000000000000, -1.000000000000000000, 0.000000000000000000 ) ) ;
#3813 = AXIS2_PLACEMENT_3D ( 'NONE', #338, #400, #466 ) ;
#3814 = ORIENTED_EDGE ( 'NONE', *, *, #12845, .T. ) ;
#3815 = AXIS2_PLACEMENT_3D ( 'NONE', #11376, #8446, #4488 ) ;
#3816 = CARTESIAN_POINT ( 'NONE',  ( -239.6374854870928175, -1.945441273133328375, 11.84125337029676395 ) ) ;
#3817 = EDGE_LOOP ( 'NONE', ( #5317, #11371 ) ) ;
#3818 = ORIENTED_EDGE ( 'NONE', *, *, #8894, .F. ) ;
#3819 = CARTESIAN_POINT ( 'NONE',  ( 240.1157413331997361, -2.212437690467188744, 2.712157915437692246 ) ) ;
#3820 = ORIENTED_EDGE ( 'NONE', *, *, #7611, .T. ) ;
#3821 = DIRECTION ( 'NONE',  ( 0.000000000000000000, 0.000000000000000000, 1.000000000000000000 ) ) ;
#3822 =( REPRESENTATION_RELATIONSHIP ('NONE','NONE', #12019, #5191 ) REPRESENTATION_RELATIONSHIP_WITH_TRANSFORMATION ( #2194 )SHAPE_REPRESENTATION_RELATIONSHIP( ) );
#3823 = EDGE_CURVE ( 'NONE', #8455, #10237, #8242, .T. ) ;
#3824 = CARTESIAN_POINT ( 'NONE',  ( -34.10614053579494964, 20.08915143303473982, -258.8746690718934929 ) ) ;
#3825 = CIRCLE ( 'NONE', #11718, 1.949999999999999734 ) ;
#3826 = DIRECTION ( 'NONE',  ( 0.000000000000000000, 0.000000000000000000, 1.000000000000000000 ) ) ;
#3827 = SURFACE_SIDE_STYLE ('',( #9828 ) ) ;
#3828 = ORIENTED_EDGE ( 'NONE', *, *, #9998, .F. ) ;
#3829 = CARTESIAN_POINT ( 'NONE',  ( -159.3442861576697283, -29.00000000000000000, -192.8974817588416499 ) ) ;
#3830 = ORIENTED_EDGE ( 'NONE', *, *, #12015, .T. ) ;
#3831 = CARTESIAN_POINT ( 'NONE',  ( 0.000000000000000000, -2.957522019940860139E-14, 0.000000000000000000 ) ) ;
#3832 = ORIENTED_EDGE ( 'NONE', *, *, #6725, .T. ) ;
#3833 = CARTESIAN_POINT ( 'NONE',  ( 240.2193860685933942, -2.381856054525893551, -2.564741263598352639 ) ) ;
#3834 = AXIS2_PLACEMENT_3D ( 'NONE', #3114, #5186, #9067 ) ;
#3835 = CARTESIAN_POINT ( 'NONE',  ( 197.8197553893915028, 18.00000000000000000, -57.77553482998991541 ) ) ;
#3836 = CARTESIAN_POINT ( 'NONE',  ( -293.0608542803120145, -30.00000000000000000, 6.485521991431936861 ) ) ;
#3837 = ADVANCED_FACE ( 'NONE', ( #11369 ), #1611, .F. ) ;
#3838 = LINE ( 'NONE', #8779, #5694 ) ;
#3839 = CARTESIAN_POINT ( 'NONE',  ( -158.7026972336038284, 20.08915143297736705, 206.8203823583187386 ) ) ;
#3840 = AXIS2_PLACEMENT_3D ( 'NONE', #9723, #3534, #747 ) ;
#3841 = CARTESIAN_POINT ( 'NONE',  ( -243.8618317092116285, -8.020662184074483392, 8.926546576192178506 ) ) ;
#3842 = CARTESIAN_POINT ( 'NONE',  ( -239.1349169580540206, 1.405155701076436392, -11.91743587425622586 ) ) ;
#3843 = ORIENTED_EDGE ( 'NONE', *, *, #5661, .T. ) ;
#3844 = DIRECTION ( 'NONE',  ( 0.000000000000000000, 0.9998057603070480415, -0.01970892327970899874 ) ) ;
#3845 = CARTESIAN_POINT ( 'NONE',  ( -159.6627199829248696, -25.00000000000000000, -193.2829683330999728 ) ) ;
#3846 = EDGE_LOOP ( 'NONE', ( #6564, #7607, #10496, #11228 ) ) ;
#3847 = ADVANCED_FACE ( 'NONE', ( #10294 ), #10122, .T. ) ;
#3848 = VERTEX_POINT ( 'NONE', #1232 ) ;
#3849 = ADVANCED_FACE ( 'NONE', ( #5293 ), #11407, .F. ) ;
#3850 = CARTESIAN_POINT ( 'NONE',  ( -249.7825649082131747, -11.59499477627102415, -1.902498381831638108 ) ) ;
#3851 = VERTEX_POINT ( 'NONE', #7429 ) ;
#3852 = CARTESIAN_POINT ( 'NONE',  ( 247.9906035370026984, 20.55460285091836070, -84.20717312441868785 ) ) ;
#3853 = CARTESIAN_POINT ( 'NONE',  ( -289.8128292627096130, -28.60000000000000142, 10.41748504886635907 ) ) ;
#3854 = CYLINDRICAL_SURFACE ( 'NONE', #1513, 230.0000000000000000 ) ;
#3855 = DIRECTION ( 'NONE',  ( -0.000000000000000000, 1.000000000000000000, 0.000000000000000000 ) ) ;
#3856 = AXIS2_PLACEMENT_3D ( 'NONE', #8112, #4034, #909 ) ;
#3857 = ORIENTED_EDGE ( 'NONE', *, *, #4405, .T. ) ;
#3858 = CARTESIAN_POINT ( 'NONE',  ( 0.000000000000000000, 9.830508068699479907, 0.000000000000000000 ) ) ;
#3859 = DIRECTION ( 'NONE',  ( -0.9063077870366467170, 0.000000000000000000, -0.4226182617407064912 ) ) ;
#3860 = LINE ( 'NONE', #6007, #3496 ) ;
#3861 = CONTEXT_DEPENDENT_SHAPE_REPRESENTATION ( #3541, #9107 ) ;
#3862 = EDGE_CURVE ( 'NONE', #11555, #2690, #7053, .T. ) ;
#3863 = EDGE_CURVE ( 'NONE', #1648, #4880, #5091, .T. ) ;
#3864 =( REPRESENTATION_RELATIONSHIP ('NONE','NONE', #12019, #182 ) REPRESENTATION_RELATIONSHIP_WITH_TRANSFORMATION ( #12179 )SHAPE_REPRESENTATION_RELATIONSHIP( ) );
#3865 = CARTESIAN_POINT ( 'NONE',  ( -229.7197800013692017, -3.900097070943512545, -11.35015525795997426 ) ) ;
#3866 = EDGE_LOOP ( 'NONE', ( #8483, #5014, #9616, #3680 ) ) ;
#3867 = ORIENTED_EDGE ( 'NONE', *, *, #9567, .T. ) ;
#3868 = CIRCLE ( 'NONE', #7283, 5.500000000000007994 ) ;
#3869 = DIRECTION ( 'NONE',  ( 0.6368676505102707219, 0.000000000000000000, 0.7709731485165535192 ) ) ;
#3870 = CARTESIAN_POINT ( 'NONE',  ( 0.000000000000000000, 0.000000000000000000, 250.0000000000000000 ) ) ;
#3871 = EDGE_CURVE ( 'NONE', #2079, #11697, #10545, .T. ) ;
#3872 = CIRCLE ( 'NONE', #5579, 250.1999999999999602 ) ;
#3873 = CARTESIAN_POINT ( 'NONE',  ( 115.5625104413773983, 20.79694577638496966, -234.3927740979615066 ) ) ;
#3874 = LINE ( 'NONE', #2865, #711 ) ;
#3875 = CARTESIAN_POINT ( 'NONE',  ( 0.000000000000000000, 0.000000000000000000, 0.000000000000000000 ) ) ;
#3876 = CIRCLE ( 'NONE', #9426, 248.1666666666679930 ) ;
#3877 = CARTESIAN_POINT ( 'NONE',  ( -245.3834146150771574, -8.931379171322292976, 7.634986101120779800 ) ) ;
#3878 = CONTEXT_DEPENDENT_SHAPE_REPRESENTATION ( #12996, #6980 ) ;
#3879 = ORIENTED_EDGE ( 'NONE', *, *, #1750, .T. ) ;
#3880 = CIRCLE ( 'NONE', #4512, 6.500000000000005329 ) ;
#3881 = CARTESIAN_POINT ( 'NONE',  ( 3.073555866996735681E-14, 24.99999999999995737, 250.3823410207189966 ) ) ;
#3882 = DIRECTION ( 'NONE',  ( 8.659560562354926695E-17, 0.7071067811865480168, -0.7071067811865470176 ) ) ;
#3883 = ORIENTED_EDGE ( 'NONE', *, *, #1321, .F. ) ;
#3884 = ORIENTED_EDGE ( 'NONE', *, *, #8821, .T. ) ;
#3885 = DIRECTION ( 'NONE',  ( 0.000000000000000000, 1.000000000000000000, 0.000000000000000000 ) ) ;
#3886 = ORIENTED_EDGE ( 'NONE', *, *, #755, .F. ) ;
#3887 = PRODUCT_DEFINITION_SHAPE ( 'NONE', 'NONE',  #13161 ) ;
#3888 = CONICAL_SURFACE ( 'NONE', #281, 6.500000000000005329, 0.7853981633974476129 ) ;
#3889 = DIRECTION ( 'NONE',  ( 0.000000000000000000, 0.000000000000000000, 1.000000000000000000 ) ) ;
#3890 = CONICAL_SURFACE ( 'NONE', #3457, 6.500000000000005329, 0.7853981633974476129 ) ;
#3891 = CARTESIAN_POINT ( 'NONE',  ( -34.10614053585819505, 20.08915143303038775, 258.8746690719034973 ) ) ;
#3892 = CARTESIAN_POINT ( 'NONE',  ( -239.5448319055423099, -1.867756360462773602, -11.85375772759396718 ) ) ;
#3893 =( NAMED_UNIT ( * ) PLANE_ANGLE_UNIT ( ) SI_UNIT ( $, .RADIAN. ) );
#3894 = ORIENTED_EDGE ( 'NONE', *, *, #3533, .F. ) ;
#3895 = DIRECTION ( 'NONE',  ( 0.000000000000000000, 1.000000000000000000, 0.000000000000000000 ) ) ;
#3896 = AXIS2_PLACEMENT_3D ( 'NONE', #5802, #11675, #6543 ) ;
#3897 = AXIS2_PLACEMENT_3D ( 'NONE', #3554, #5368, #7627 ) ;
#3898 = AXIS2_PLACEMENT_3D ( 'NONE', #7379, #2177, #3234 ) ;
#3899 = EDGE_LOOP ( 'NONE', ( #1066, #4148, #7825, #2905, #3775, #3602, #2502, #5828, #1215, #10412 ) ) ;
#3900 = AXIS2_PLACEMENT_3D ( 'NONE', #5360, #9430, #2483 ) ;
#3901 = CARTESIAN_POINT ( 'NONE',  ( -239.3871160943602661, 1.704640309878053150, 11.62580261321480535 ) ) ;
#3902 = EDGE_LOOP ( 'NONE', ( #10603, #5641, #12180, #12915 ) ) ;
#3903 = PLANE ( 'NONE',  #12797 ) ;
#3904 = DIRECTION ( 'NONE',  ( 0.000000000000000000, 0.000000000000000000, 1.000000000000000000 ) ) ;
#3905 = CARTESIAN_POINT ( 'NONE',  ( 239.1683641398503255, 0.9613626713097240817, 3.365491595542490444 ) ) ;
#3906 = CARTESIAN_POINT ( 'NONE',  ( 0.000000000000000000, -20.00000000000000000, 0.000000000000000000 ) ) ;
#3907 = CIRCLE ( 'NONE', #8597, 2.900000000000000355 ) ;
#3908 = DIRECTION ( 'NONE',  ( 0.000000000000000000, 0.000000000000000000, -1.000000000000000000 ) ) ;
#3909 = CARTESIAN_POINT ( 'NONE',  ( -242.3288872984456361, -6.653385920035336909, 9.986615906358528250 ) ) ;
#3910 = CARTESIAN_POINT ( 'NONE',  ( -206.9952515782967168, 20.79694577634646535, -158.8368823490026500 ) ) ;
#3911 = ITEM_DEFINED_TRANSFORMATION ( 'NONE', 'NONE', #12728,  #805 ) ;
#3912 = EDGE_LOOP ( 'NONE', ( #9683, #971, #10820, #232 ) ) ;
#3913 = CARTESIAN_POINT ( 'NONE',  ( 197.8197553893920144, 19.00000000000000000, 58.77553482998850853 ) ) ;
#3914 = ORIENTED_EDGE ( 'NONE', *, *, #370, .F. ) ;
#3915 = EDGE_CURVE ( 'NONE', #6766, #3428, #5011, .T. ) ;
#3916 = EDGE_CURVE ( 'NONE', #8050, #2022, #9905, .T. ) ;
#3917 = VECTOR ( 'NONE', #12828, 1000.000000000000000 ) ;
#3918 = ORIENTED_EDGE ( 'NONE', *, *, #10806, .F. ) ;
#3919 = CARTESIAN_POINT ( 'NONE',  ( -249.6587182942291179, -11.13358978280005118, -3.756204109176177752 ) ) ;
#3920 = ORIENTED_EDGE ( 'NONE', *, *, #8649, .T. ) ;
#3921 = CARTESIAN_POINT ( 'NONE',  ( -67.76049180359858326, 20.55460285124812359, -252.9796497731095997 ) ) ;
#3922 = CARTESIAN_POINT ( 'NONE',  ( -248.3022220570269099, 9.870789006252802977, -6.824104388866809145 ) ) ;
#3923 = DIRECTION ( 'NONE',  ( 0.000000000000000000, -1.000000000000000000, 0.000000000000000000 ) ) ;
#3924 = DIRECTION ( 'NONE',  ( 0.000000000000000000, -1.000000000000000000, 0.000000000000000000 ) ) ;
#3925 = CARTESIAN_POINT ( 'NONE',  ( -246.2633612349185626, 9.321506464660762603, 7.557087659995063156 ) ) ;
#3926 = CONICAL_SURFACE ( 'NONE', #9669, 6.500000000000000888, 0.7853981633974617127 ) ;
#3927 = AXIS2_PLACEMENT_3D ( 'NONE', #4398, #8289, #5412 ) ;
#3928 = PRESENTATION_STYLE_ASSIGNMENT (( #5871 ) ) ;
#3929 = DIRECTION ( 'NONE',  ( -0.5887335932212889311, 0.5538822189107472926, -0.5887335932212951484 ) ) ;
#3930 = CARTESIAN_POINT ( 'NONE',  ( -229.9952077895577247, -11.65587983266546424, 1.533898002187394916 ) ) ;
#3931 = CARTESIAN_POINT ( 'NONE',  ( -229.9710968621332654, -11.43322075889305189, -3.663687894926668687 ) ) ;
#3932 = ORIENTED_EDGE ( 'NONE', *, *, #11867, .F. ) ;
#3933 = VERTEX_POINT ( 'NONE', #4610 ) ;
#3934 = AXIS2_PLACEMENT_3D ( 'NONE', #7862, #10182, #6130 ) ;
#3935 = CARTESIAN_POINT ( 'NONE',  ( -185.9653539489998195, -29.00000000000000000, -225.1241593668329699 ) ) ;
#3936 = DIRECTION ( 'NONE',  ( 0.000000000000000000, 0.000000000000000000, -1.000000000000000000 ) ) ;
#3937 = DIRECTION ( 'NONE',  ( 0.000000000000000000, 1.000000000000000000, 0.000000000000000000 ) ) ;
#3938 = EDGE_CURVE ( 'NONE', #5812, #9614, #5869, .T. ) ;
#3939 = CARTESIAN_POINT ( 'NONE',  ( 252.4341100445949735, 20.79694577582237613, 67.61424742981928659 ) ) ;
#3940 = EDGE_CURVE ( 'NONE', #9649, #169, #9615, .T. ) ;
#3941 = FACE_OUTER_BOUND ( 'NONE', #9072, .T. ) ;
#3942 = DIRECTION ( 'NONE',  ( -0.4226182617406912256, 0.000000000000000000, -0.9063077870366540445 ) ) ;
#3943 = CARTESIAN_POINT ( 'NONE',  ( -242.7734209792739364, -7.097132674162740962, 9.364576600943349760 ) ) ;
#3944 = TOROIDAL_SURFACE ( 'NONE', #1610, 261.5294117647060261, 2.000000000000000000 ) ;
#3945 = ITEM_DEFINED_TRANSFORMATION ( 'NONE', 'NONE', #606,  #805 ) ;
#3946 = ORIENTED_EDGE ( 'NONE', *, *, #846, .F. ) ;
#3947 = AXIS2_PLACEMENT_3D ( 'NONE', #3831, #4964, #5027 ) ;
#3948 = DIRECTION ( 'NONE',  ( 1.000000000000000000, 0.000000000000000000, 0.000000000000000000 ) ) ;
#3949 = CARTESIAN_POINT ( 'NONE',  ( -239.0387908882599106, -1.252775419848246363, 11.93442892173632330 ) ) ;
#3950 = ORIENTED_EDGE ( 'NONE', *, *, #11328, .T. ) ;
#3951 = ORIENTED_EDGE ( 'NONE', *, *, #3767, .T. ) ;
#3952 = ADVANCED_BREP_SHAPE_REPRESENTATION ( '', ( #10422, #805 ), #1657 ) ;
#3953 = DIRECTION ( 'NONE',  ( 0.4503334343941595153, -0.7071067811865431318, 0.5451603414288016536 ) ) ;
#3954 = VERTEX_POINT ( 'NONE', #3415 ) ;
#3955 = CARTESIAN_POINT ( 'NONE',  ( -159.3442861576697283, 19.00000000000000000, -192.8974817588417352 ) ) ;
#3956 = CARTESIAN_POINT ( 'NONE',  ( -34.18476129408180242, 19.96883745937779864, 259.4723857443443080 ) ) ;
#3957 = EDGE_CURVE ( 'NONE', #468, #12455, #7562, .T. ) ;
#3958 = CARTESIAN_POINT ( 'NONE',  ( -238.6985546646470198, 6.516754929249349828E-09, -12.00000000011316459 ) ) ;
#3959 = CARTESIAN_POINT ( 'NONE',  ( -246.8900737811224815, 9.535158802951487544, 6.866190026894644305 ) ) ;
#3960 = ORIENTED_EDGE ( 'NONE', *, *, #2991, .T. ) ;
#3961 = B_SPLINE_CURVE_WITH_KNOTS ( 'NONE', 3,
 ( #11679, #7668, #11744, #6685, #1541, #5809, #4795, #2596, #12606, #10738, #9665, #8805, #2536, #5608, #547, #9796, #1609, #609, #3469, #4728, #8670, #12869, #11815, #7544, #2471, #6548, #7799, #11871, #2719, #6810, #10601, #10868, #5040, #3799, #12385, #2112, #5175, #3170, #1120, #7253, #2974, #4245, #11243, #8126, #10243, #4178, #8324, #9186, #10374, #2249, #11938, #8195, #12256, #11115, #3239, #12314, #3106, #7183, #1985, #7320, #11319, #7055, #1248, #5108, #62, #6059, #12932, #4115, #6324, #11387, #12186, #10113, #6262, #9254, #459, #6189, #9114, #8869, #10171, #985, #129, #1050, #7866 ),
 .UNSPECIFIED., .F., .F.,
 ( 4, 2, 1, 1, 1, 2, 2, 2, 1, 1, 1, 1, 2, 2, 2, 2, 1, 1, 1, 1, 2, 2, 2, 2, 1, 1, 1, 2, 2, 2, 1, 1, 1, 1, 2, 2, 2, 2, 1, 1, 1, 2, 2, 2, 1, 1, 2, 2, 2, 1, 1, 2, 2, 4 ),
 ( 0.000000000000000000, 0.06250000000013644641, 0.09375000000020380919, 0.1093750000002384343, 0.1171875000002566974, 0.1210937500002668976, 0.1250000000002770839, 0.1875000000004268808, 0.2187500000005017098, 0.2343750000005390688, 0.2421875000005577483, 0.2460937500005684342, 0.2480468750005739020, 0.2500000000005793699, 0.3125000000007500667, 0.3437500000008369416, 0.3593750000008821277, 0.3671875000009031109, 0.3710937500009120482, 0.3730468750009181544, 0.3740234375009196532, 0.3750000000009210965, 0.4375000000009141021, 0.4687500000009104939, 0.4843750000009103274, 0.4921875000009120482, 0.4960937500009112155, 0.4980468750009108270, 0.5000000000009103829, 0.5625000000007968071, 0.5937500000007399636, 0.6093750000007095435, 0.6171875000006963319, 0.6210937500006896705, 0.6230468750006864509, 0.6250000000006831202, 0.6875000000006470380, 0.7187500000006311618, 0.7343750000006259437, 0.7421875000006260548, 0.7460937500006262768, 0.7480468750006264989, 0.7500000000006266099, 0.7812500000005730971, 0.7968750000005464518, 0.8046875000005330181, 0.8085937500005236922, 0.8125000000005143663, 0.8437500000004438672, 0.8593750000004061196, 0.8671875000003899103, 0.8710937500003791412, 0.8750000000003683720, 1.000000000000000000 ),
 .UNSPECIFIED. ) ;
#3962 = DIRECTION ( 'NONE',  ( -0.6368676505102696117, 0.000000000000000000, -0.7709731485165545184 ) ) ;
#3963 = ORIENTED_EDGE ( 'NONE', *, *, #5644, .F. ) ;
#3964 = CARTESIAN_POINT ( 'NONE',  ( -245.2595250062178707, 8.869312995476704486, -7.707186825661166196 ) ) ;
#3965 = ORIENTED_EDGE ( 'NONE', *, *, #2252, .T. ) ;
#3966 = DIRECTION ( 'NONE',  ( -0.000000000000000000, -1.000000000000000000, 0.000000000000000000 ) ) ;
#3967 = DIRECTION ( 'NONE',  ( 0.4503334343941555740, 0.7071067811865490160, 0.5451603414287971017 ) ) ;
#3968 = CARTESIAN_POINT ( 'NONE',  ( 239.5387464294004474, 1.581210111871798940, 3.124650851984021038 ) ) ;
#3969 = DIRECTION ( 'NONE',  ( 0.000000000000000000, 0.000000000000000000, 1.000000000000000000 ) ) ;
#3970 = LINE ( 'NONE', #9045, #4137 ) ;
#3971 = CARTESIAN_POINT ( 'NONE',  ( -240.5058532487308582, -3.857938722311311075, 11.36295048183375300 ) ) ;
#3972 = CARTESIAN_POINT ( 'NONE',  ( -239.4909294952468315, 1.818763105859342755, -11.86135880463733727 ) ) ;
#3973 = UNCERTAINTY_MEASURE_WITH_UNIT (LENGTH_MEASURE( 1.000000000000000082E-05 ), #8905, 'distance_accuracy_value', 'NONE');
#3974 = CONTEXT_DEPENDENT_SHAPE_REPRESENTATION ( #1149, #10943 ) ;
#3975 = VERTEX_POINT ( 'NONE', #1495 ) ;
#3976 = DIRECTION ( 'NONE',  ( -0.000000000000000000, -1.000000000000000000, 0.000000000000000000 ) ) ;
#3977 = ORIENTED_EDGE ( 'NONE', *, *, #8203, .T. ) ;
#3978 = CARTESIAN_POINT ( 'NONE',  ( -249.2754563888361758, -10.50954084450015991, 5.254718384043918000 ) ) ;
#3979 = ORIENTED_EDGE ( 'NONE', *, *, #7505, .T. ) ;
#3980 = CARTESIAN_POINT ( 'NONE',  ( -247.4557548106230058, 20.79694577606145600, -84.02568524181840814 ) ) ;
#3981 = DIRECTION ( 'NONE',  ( -0.000000000000000000, -1.000000000000000000, 0.000000000000000000 ) ) ;
#3982 = DIRECTION ( 'NONE',  ( 0.000000000000000000, -0.7071067811865489050, -0.7071067811865460184 ) ) ;
#3983 = CARTESIAN_POINT ( 'NONE',  ( -246.7886136447417300, -9.502664450157794818, -6.911022174141807639 ) ) ;
#3984 = AXIS2_PLACEMENT_3D ( 'NONE', #12800, #12775, #7837 ) ;
#3985 = EDGE_CURVE ( 'NONE', #11069, #169, #12737, .T. ) ;
#3986 = CARTESIAN_POINT ( 'NONE',  ( -244.6090102851887593, 8.514624253206315885, 8.455955369777946373 ) ) ;
#3987 = ADVANCED_FACE ( 'NONE', ( #11701 ), #10613, .F. ) ;
#3988 = FACE_OUTER_BOUND ( 'NONE', #3761, .T. ) ;
#3989 = DIRECTION ( 'NONE',  ( 0.08715574274766850482, 0.000000000000000000, -0.9961946980917446570 ) ) ;
#3990 = DIRECTION ( 'NONE',  ( 1.000000000000000000, 0.000000000000000000, 0.000000000000000000 ) ) ;
#3991 = PRODUCT_DEFINITION_SHAPE ( 'NONE', 'NONE',  #13127 ) ;
#3992 = DIRECTION ( 'NONE',  ( 0.000000000000000000, 0.000000000000000000, 1.000000000000000000 ) ) ;
#3993 = ORIENTED_EDGE ( 'NONE', *, *, #3531, .T. ) ;
#3994 = ORIENTED_EDGE ( 'NONE', *, *, #12176, .F. ) ;
#3995 = DIRECTION ( 'NONE',  ( 0.4503334343941626794, -0.7071067811865380248, 0.5451603414288055394 ) ) ;
#3996 = CARTESIAN_POINT ( 'NONE',  ( 229.9000000000000057, 4.038376339049584374, 2.818069648572310459 ) ) ;
#3997 = CYLINDRICAL_SURFACE ( 'NONE', #10007, 5.500000000000005329 ) ;
#3998 = CIRCLE ( 'NONE', #5940, 6.499999999999999112 ) ;
#3999 = CARTESIAN_POINT ( 'NONE',  ( -181.8257142206830679, -30.00000000000000000, -220.1128339014753692 ) ) ;
#4000 = AXIS2_PLACEMENT_3D ( 'NONE', #2607, #1618, #5683 ) ;
#4001 = DIRECTION ( 'NONE',  ( -0.000000000000000000, -1.000000000000000000, 0.000000000000000000 ) ) ;
#4002 = DIRECTION ( 'NONE',  ( 0.5000000000000101030, 0.000000000000000000, -0.8660254037844328234 ) ) ;
#4003 = CARTESIAN_POINT ( 'NONE',  ( -241.3417439075396373, -5.375691555202312344, 10.44818116087240512 ) ) ;
#4004 = CONTEXT_DEPENDENT_SHAPE_REPRESENTATION ( #973, #12234 ) ;
#4005 = VERTEX_POINT ( 'NONE', #1368 ) ;
#4006 = DIRECTION ( 'NONE',  ( -0.6368676505102708330, 0.000000000000000000, -0.7709731485165536302 ) ) ;
#4007 = CARTESIAN_POINT ( 'NONE',  ( -239.4329164336750466, -1.762478856070534006, 11.86986396151673517 ) ) ;
#4008 = ORIENTED_EDGE ( 'NONE', *, *, #12259, .F. ) ;
#4009 = VECTOR ( 'NONE', #7382, 1000.000000000000000 ) ;
#4010 = ORIENTED_EDGE ( 'NONE', *, *, #6649, .F. ) ;
#4011 = EDGE_CURVE ( 'NONE', #11136, #8469, #4483, .T. ) ;
#4012 = CIRCLE ( 'NONE', #9989, 5.500000000000007994 ) ;
#4013 = EDGE_CURVE ( 'NONE', #12433, #8176, #11476, .T. ) ;
#4014 = CARTESIAN_POINT ( 'NONE',  ( 0.000000000000000000, 25.00000000000000000, 0.000000000000000000 ) ) ;
#4015 = DIRECTION ( 'NONE',  ( -0.000000000000000000, -1.000000000000000000, 0.000000000000000000 ) ) ;
#4016 = CIRCLE ( 'NONE', #8916, 5.500000000000005329 ) ;
#4017 = VECTOR ( 'NONE', #4212, 1000.000000000000000 ) ;
#4018 = DIRECTION ( 'NONE',  ( 0.6368676505102716101, 0.000000000000000000, 0.7709731485165527420 ) ) ;
#4019 = AXIS2_PLACEMENT_3D ( 'NONE', #12858, #3651, #11859 ) ;
#4020 = CARTESIAN_POINT ( 'NONE',  ( -1.009475258464312158E-12, 20.08915143297736350, 260.5542428351129729 ) ) ;
#4021 = CARTESIAN_POINT ( 'NONE',  ( -239.0745754881768050, -1.312373183774685703, -11.92802719768877573 ) ) ;
#4022 = DIRECTION ( 'NONE',  ( 0.9961946980917455452, 0.000000000000000000, 0.08715574274765836016 ) ) ;
#4023 = CARTESIAN_POINT ( 'NONE',  ( -246.2885828769054228, 9.329251171726635761, 7.144935789750891608 ) ) ;
#4024 = AXIS2_PLACEMENT_3D ( 'NONE', #9043, #3159, #7244 ) ;
#4025 = ORIENTED_EDGE ( 'NONE', *, *, #2885, .F. ) ;
#4026 = FACE_OUTER_BOUND ( 'NONE', #6436, .T. ) ;
#4027 = EDGE_LOOP ( 'NONE', ( #768, #1048 ) ) ;
#4028 = AXIS2_PLACEMENT_3D ( 'NONE', #8020, #887, #11013 ) ;
#4029 = FACE_OUTER_BOUND ( 'NONE', #1380, .T. ) ;
#4030 = VERTEX_POINT ( 'NONE', #9681 ) ;
#4031 = EDGE_CURVE ( 'NONE', #13016, #926, #7754, .T. ) ;
#4032 = CIRCLE ( 'NONE', #5315, 6.500000000000005329 ) ;
#4033 = DIRECTION ( 'NONE',  ( 0.6368676505102707219, 0.000000000000000000, 0.7709731485165535192 ) ) ;
#4034 = DIRECTION ( 'NONE',  ( 0.000000000000000000, 1.000000000000000000, 0.000000000000000000 ) ) ;
#4035 = FACE_OUTER_BOUND ( 'NONE', #7495, .T. ) ;
#4036 = CARTESIAN_POINT ( 'NONE',  ( 234.3487510399341716, 0.000000000000000000, 0.000000000000000000 ) ) ;
#4037 = AXIS2_PLACEMENT_3D ( 'NONE', #1322, #5388, #4502 ) ;
#4038 = EDGE_CURVE ( 'NONE', #1970, #4613, #12536, .T. ) ;
#4039 = CARTESIAN_POINT ( 'NONE',  ( 294.1869546181097235, -19.00000000000000000, 31.92980917095290749 ) ) ;
#4040 = CARTESIAN_POINT ( 'NONE',  ( 0.000000000000000000, 30.00000000000000000, 208.0000000000000000 ) ) ;
#4041 = CARTESIAN_POINT ( 'NONE',  ( -239.4341775791918394, 1.763735210516577778, -11.86967692145091213 ) ) ;
#4042 = ORIENTED_EDGE ( 'NONE', *, *, #11276, .F. ) ;
#4043 = CARTESIAN_POINT ( 'NONE',  ( -238.9989076695733559, -1.159495732441587768, -11.69268798842454160 ) ) ;
#4044 = AXIS2_PLACEMENT_3D ( 'NONE', #6478, #11673, #9715 ) ;
#4045 = ORIENTED_EDGE ( 'NONE', *, *, #2051, .T. ) ;
#4046 = CARTESIAN_POINT ( 'NONE',  ( -249.7994671776788209, 11.75014634418644377, -0.3782187742944450037 ) ) ;
#4047 = CARTESIAN_POINT ( 'NONE',  ( 0.000000000000000000, 1.848645179567965036, 0.000000000000000000 ) ) ;
#4048 = AXIS2_PLACEMENT_3D ( 'NONE', #6870, #7795, #10996 ) ;
#4049 = CARTESIAN_POINT ( 'NONE',  ( -249.7095932324938872, -11.27773618749138684, 3.298468584332664655 ) ) ;
#4050 = ORIENTED_EDGE ( 'NONE', *, *, #1006, .T. ) ;
#4051 = CARTESIAN_POINT ( 'NONE',  ( 260.7745447061710138, 20.79694577634651509, -17.06760680878044667 ) ) ;
#4052 = CARTESIAN_POINT ( 'NONE',  ( -247.0023889698559287, 9.573823397979071004, -7.235426327079722775 ) ) ;
#4053 = CARTESIAN_POINT ( 'NONE',  ( -239.8125244181988762, 2.098251439821959607, 11.56389750601951327 ) ) ;
#4054 = CONICAL_SURFACE ( 'NONE', #8737, 249.7999999999999829, 0.7853981633974066456 ) ;
#4055 = CARTESIAN_POINT ( 'NONE',  ( -247.1459274944737103, -9.611803614974679277, -6.758488902612981519 ) ) ;
#4056 = CARTESIAN_POINT ( 'NONE',  ( -243.4562500152165399, 7.708554438554969579, 9.196640587735709360 ) ) ;
#4057 = CIRCLE ( 'NONE', #9521, 231.0000000000000000 ) ;
#4058 = DIRECTION ( 'NONE',  ( 0.000000000000000000, 0.000000000000000000, -1.000000000000000000 ) ) ;
#4059 = CARTESIAN_POINT ( 'NONE',  ( 32.05991134143095422, -138.4705547276867321, 26.90145978217163503 ) ) ;
#4060 = CARTESIAN_POINT ( 'NONE',  ( 0.000000000000000000, 19.00000000000000000, 0.000000000000000000 ) ) ;
#4061 = CYLINDRICAL_SURFACE ( 'NONE', #265, 5.500000000000005329 ) ;
#4062 = VERTEX_POINT ( 'NONE', #8567 ) ;
#4063 = ORIENTED_EDGE ( 'NONE', *, *, #4879, .T. ) ;
#4064 = EDGE_CURVE ( 'NONE', #2618, #4412, #10402, .T. ) ;
#4065 = MECHANICAL_DESIGN_GEOMETRIC_PRESENTATION_REPRESENTATION (  '', ( #2366 ), #6382 ) ;
#4066 = CARTESIAN_POINT ( 'NONE',  ( -241.2893272559581135, -5.295647553031770371, 10.48903809276563059 ) ) ;
#4067 = CARTESIAN_POINT ( 'NONE',  ( -234.1947771733725006, 20.08915143296620442, 115.4648407707744013 ) ) ;
#4068 = DIRECTION ( 'NONE',  ( 0.7709731485165535192, 0.000000000000000000, -0.6368676505102707219 ) ) ;
#4069 = VECTOR ( 'NONE', #5314, 1000.000000000000000 ) ;
#4070 = CARTESIAN_POINT ( 'NONE',  ( 6.735557395310442023E-16, 30.00000000000000000, 202.4999999999999716 ) ) ;
#4071 = DIRECTION ( 'NONE',  ( -0.000000000000000000, -1.000000000000000000, 0.000000000000000000 ) ) ;
#4072 = CIRCLE ( 'NONE', #2996, 2.000000000000001776 ) ;
#4073 = LINE ( 'NONE', #11075, #7721 ) ;
#4074 = CARTESIAN_POINT ( 'NONE',  ( 0.000000000000000000, 0.000000000000000000, 0.000000000000000000 ) ) ;
#4075 = CARTESIAN_POINT ( 'NONE',  ( -241.8128863209092856, -6.047237972655528537, 10.08137159841291997 ) ) ;
#4076 = DIRECTION ( 'NONE',  ( 0.4999999999999888978, 0.000000000000000000, 0.8660254037844450359 ) ) ;
#4077 = VERTEX_POINT ( 'NONE', #6567 ) ;
#4078 = FACE_BOUND ( 'NONE', #2342, .T. ) ;
#4079 = CARTESIAN_POINT ( 'NONE',  ( 229.9933841504430063, -3.036907577538628278, -1.754770297504167464 ) ) ;
#4080 = EDGE_LOOP ( 'NONE', ( #1925, #12945, #4780, #8872 ) ) ;
#4081 = ADVANCED_FACE ( 'NONE', ( #2426 ), #12956, .F. ) ;
#4082 = EDGE_LOOP ( 'NONE', ( #11368, #9113, #10169, #3950 ) ) ;
#4083 = EDGE_CURVE ( 'NONE', #9366, #327, #6701, .T. ) ;
#4084 = FACE_OUTER_BOUND ( 'NONE', #11700, .T. ) ;
#4085 = ORIENTED_EDGE ( 'NONE', *, *, #11847, .F. ) ;
#4086 = CIRCLE ( 'NONE', #8774, 6.500000000000005329 ) ;
#4087 = CARTESIAN_POINT ( 'NONE',  ( -259.4723857429215741, 19.96883746091132394, -34.18476129331127567 ) ) ;
#4088 = CARTESIAN_POINT ( 'NONE',  ( -239.4798992437278855, -1.808255580866046985, -11.86296839994171926 ) ) ;
#4089 = AXIS2_PLACEMENT_3D ( 'NONE', #3100, #7176, #6317 ) ;
#4090 = CARTESIAN_POINT ( 'NONE',  ( -242.8048495207236215, 7.129644030681907552, 9.341687345561288325 ) ) ;
#4091 = ADVANCED_FACE ( 'NONE', ( #1561 ), #565, .F. ) ;
#4092 = EDGE_LOOP ( 'NONE', ( #5591, #9744, #1426, #11032 ) ) ;
#4093 = CARTESIAN_POINT ( 'NONE',  ( 257.4287020129719963, 20.79694577634646535, 42.50473797389774688 ) ) ;
#4094 = CIRCLE ( 'NONE', #7291, 245.7999999999999829 ) ;
#4095 = ORIENTED_EDGE ( 'NONE', *, *, #9465, .F. ) ;
#4096 = DIRECTION ( 'NONE',  ( 0.6368676505102707219, 0.000000000000000000, 0.7709731485165536302 ) ) ;
#4097 = ORIENTED_EDGE ( 'NONE', *, *, #846, .T. ) ;
#4098 = CIRCLE ( 'NONE', #6020, 259.6078431372549744 ) ;
#4099 = CIRCLE ( 'NONE', #7094, 5.500000000000015099 ) ;
#4100 = DIRECTION ( 'NONE',  ( 0.000000000000000000, 1.000000000000000000, 0.000000000000000000 ) ) ;
#4101 = CARTESIAN_POINT ( 'NONE',  ( 240.3826708216974737, 2.772967769358989809, 2.135567781667440102 ) ) ;
#4102 = CARTESIAN_POINT ( 'NONE',  ( 239.6467530165474784, 1.711397835215433760, 3.057326063786706793 ) ) ;
#4103 = CARTESIAN_POINT ( 'NONE',  ( 239.7985776503645354, -1.848645179573700004, -2.971954070984049956 ) ) ;
#4104 = CARTESIAN_POINT ( 'NONE',  ( -233.8077470125389254, 20.08915143297736705, -115.3046144132258917 ) ) ;
#4105 = PRODUCT_DEFINITION_SHAPE ( 'NONE', 'NONE',  #13124 ) ;
#4106 = DIRECTION ( 'NONE',  ( 0.6368676505102698338, 0.000000000000000000, 0.7709731485165542964 ) ) ;
#4107 = EDGE_CURVE ( 'NONE', #3688, #9318, #1680, .T. ) ;
#4108 = ADVANCED_FACE ( 'NONE', ( #2612 ), #5077, .F. ) ;
#4109 = LINE ( 'NONE', #8190, #12039 ) ;
#4110 = ITEM_DEFINED_TRANSFORMATION ( 'NONE', 'NONE', #2291,  #805 ) ;
#4111 = ORIENTED_EDGE ( 'NONE', *, *, #11687, .F. ) ;
#4112 = FACE_BOUND ( 'NONE', #11713, .T. ) ;
#4113 = ORIENTED_EDGE ( 'NONE', *, *, #5991, .F. ) ;
#4114 = CARTESIAN_POINT ( 'NONE',  ( -249.2798997179278615, 10.51457946798599608, -5.244637040181677534 ) ) ;
#4115 = CARTESIAN_POINT ( 'NONE',  ( -246.8626574249385328, -9.530421748743428623, -7.291787928471770819 ) ) ;
#4116 = ADVANCED_FACE ( 'NONE', ( #1430 ), #7498, .F. ) ;
#4117 = CARTESIAN_POINT ( 'NONE',  ( 160.6180214586902366, -11.79660968244695951, 194.4394280558747994 ) ) ;
#4118 = ORIENTED_EDGE ( 'NONE', *, *, #2230, .F. ) ;
#4119 = CIRCLE ( 'NONE', #6040, 248.7999999999999829 ) ;
#4120 = CARTESIAN_POINT ( 'NONE',  ( -159.0697709836499882, 20.79694577635847352, 207.3438552937170130 ) ) ;
#4121 = CARTESIAN_POINT ( 'NONE',  ( -246.5457465964734638, 9.425397934458551674, -7.427386667154282307 ) ) ;
#4122 = FACE_OUTER_BOUND ( 'NONE', #3489, .T. ) ;
#4123 = CARTESIAN_POINT ( 'NONE',  ( -244.5179878651543675, -8.451416882004156861, -8.163389688603578165 ) ) ;
#4124 =( REPRESENTATION_RELATIONSHIP ('NONE','NONE', #12019, #182 ) REPRESENTATION_RELATIONSHIP_WITH_TRANSFORMATION ( #8253 )SHAPE_REPRESENTATION_RELATIONSHIP( ) );
#4125 = EDGE_CURVE ( 'NONE', #7101, #12848, #2314, .T. ) ;
#4126 = CARTESIAN_POINT ( 'NONE',  ( 24.18668477630848557, -30.00000000000000000, -294.9245348571437262 ) ) ;
#4127 = DIRECTION ( 'NONE',  ( 0.8294267566935217273, 0.5538822189107470706, -0.07256543843574986274 ) ) ;
#4128 = CARTESIAN_POINT ( 'NONE',  ( -229.7297352805116759, -3.784240722071517293, 11.15059988720178374 ) ) ;
#4129 = AXIS2_PLACEMENT_3D ( 'NONE', #7365, #2090, #5224 ) ;
#4130 = ITEM_DEFINED_TRANSFORMATION ( 'NONE', 'NONE', #9581,  #805 ) ;
#4131 = DIRECTION ( 'NONE',  ( 0.5469441386039890496, 0.000000000000000000, -0.8371691043312220470 ) ) ;
#4132 = EDGE_LOOP ( 'NONE', ( #11800, #11969 ) ) ;
#4133 = VERTEX_POINT ( 'NONE', #4742 ) ;
#4134 = CARTESIAN_POINT ( 'NONE',  ( -207.1687172315079692, 20.08915143295307004, 158.9353507253535156 ) ) ;
#4135 = FACE_OUTER_BOUND ( 'NONE', #12691, .T. ) ;
#4136 = PRODUCT_DEFINITION_SHAPE ( 'NONE', 'NONE',  #13095 ) ;
#4137 = VECTOR ( 'NONE', #8045, 1000.000000000000114 ) ;
#4138 = CARTESIAN_POINT ( 'NONE',  ( 0.000000000000000000, -2.156506209390995021, 0.000000000000000000 ) ) ;
#4139 = CARTESIAN_POINT ( 'NONE',  ( 227.3999999999999773, 4.550331206106116078, 2.508881407069060376 ) ) ;
#4140 = CARTESIAN_POINT ( 'NONE',  ( 161.8917567597108018, -22.00000000000000000, 195.9813743529078920 ) ) ;
#4141 = CARTESIAN_POINT ( 'NONE',  ( -210.0000000000000000, 28.60000000000000142, 0.000000000000000000 ) ) ;
#4142 = DIRECTION ( 'NONE',  ( 0.2588190451025078609, 0.000000000000000000, 0.9659258262890717539 ) ) ;
#4143 = CARTESIAN_POINT ( 'NONE',  ( -243.1580368189675028, -7.448595192430751410, 9.087405006325091961 ) ) ;
#4144 = ORIENTED_EDGE ( 'NONE', *, *, #12991, .F. ) ;
#4145 = CARTESIAN_POINT ( 'NONE',  ( -0.000000000000000000, -11.79660968244695951, 0.000000000000000000 ) ) ;
#4146 = AXIS2_PLACEMENT_3D ( 'NONE', #11600, #6790, #1720 ) ;
#4147 = CARTESIAN_POINT ( 'NONE',  ( 0.000000000000000000, 21.94174202707280941, 251.2912898646363828 ) ) ;
#4148 = ORIENTED_EDGE ( 'NONE', *, *, #4249, .T. ) ;
#4149 = ORIENTED_EDGE ( 'NONE', *, *, #9689, .T. ) ;
#4150 = CYLINDRICAL_SURFACE ( 'NONE', #12112, 5.500000000000015099 ) ;
#4151 = DIRECTION ( 'NONE',  ( -0.7709731485165536302, 0.000000000000000000, 0.6368676505102706109 ) ) ;
#4152 = CARTESIAN_POINT ( 'NONE',  ( 260.5542428351129729, 20.08915143297735284, 17.05314194231024771 ) ) ;
#4153 = VECTOR ( 'NONE', #7074, 1000.000000000000114 ) ;
#4154 = CARTESIAN_POINT ( 'NONE',  ( -238.7337772397934259, -0.4297369727470538581, -11.99275889149802055 ) ) ;
#4155 = DIRECTION ( 'NONE',  ( -0.08715574274765836016, 0.000000000000000000, 0.9961946980917455452 ) ) ;
#4156 = AXIS2_PLACEMENT_3D ( 'NONE', #11227, #12623, #11830 ) ;
#4157 = CARTESIAN_POINT ( 'NONE',  ( -244.2871807289265575, 8.304201005827847482, 8.312831357947803923 ) ) ;
#4158 = ADVANCED_FACE ( 'NONE', ( #6895 ), #8884, .F. ) ;
#4159 = EDGE_CURVE ( 'NONE', #12455, #1965, #692, .T. ) ;
#4160 = ORIENTED_EDGE ( 'NONE', *, *, #4320, .F. ) ;
#4161 = DIRECTION ( 'NONE',  ( -0.000000000000000000, -1.000000000000000000, 0.000000000000000000 ) ) ;
#4162 = ORIENTED_EDGE ( 'NONE', *, *, #8682, .T. ) ;
#4163 = CARTESIAN_POINT ( 'NONE',  ( -197.8197553893924976, 18.00000000000000000, -57.77553482998720824 ) ) ;
#4164 = ORIENTED_EDGE ( 'NONE', *, *, #39, .T. ) ;
#4165 = ORIENTED_EDGE ( 'NONE', *, *, #11572, .F. ) ;
#4166 = AXIS2_PLACEMENT_3D ( 'NONE', #2732, #4740, #10812 ) ;
#4167 = VECTOR ( 'NONE', #7202, 1000.000000000000000 ) ;
#4168 = DIRECTION ( 'NONE',  ( 0.7071067811865480168, -0.7069694329824850465, 0.01393631330096772175 ) ) ;
#4169 = SURFACE_STYLE_USAGE ( .BOTH. , #11436 ) ;
#4170 = CARTESIAN_POINT ( 'NONE',  ( 239.3359268382297387, 1.289900281958762385, 3.253812819694583691 ) ) ;
#4171 = DIRECTION ( 'NONE',  ( 0.000000000000000000, 0.000000000000000000, 1.000000000000000000 ) ) ;
#4172 = CARTESIAN_POINT ( 'NONE',  ( -91.83222442980213884, 20.08915143297737060, -243.9837273761029621 ) ) ;
#4173 = DIRECTION ( 'NONE',  ( 0.000000000000000000, 1.000000000000000000, 0.000000000000000000 ) ) ;
#4174 = CONTEXT_DEPENDENT_SHAPE_REPRESENTATION ( #12801, #2237 ) ;
#4175 = ORIENTED_EDGE ( 'NONE', *, *, #12991, .T. ) ;
#4176 = ORIENTED_EDGE ( 'NONE', *, *, #5583, .T. ) ;
#4177 = CARTESIAN_POINT ( 'NONE',  ( 0.000000000000000000, 18.00000000000000000, 0.000000000000000000 ) ) ;
#4178 = CARTESIAN_POINT ( 'NONE',  ( -244.2419534911824144, -8.283406880650625581, -8.682674419792185461 ) ) ;
#4179 = CARTESIAN_POINT ( 'NONE',  ( 83.79436865282340818, 20.08915143297736705, -246.8597181602070805 ) ) ;
#4180 = VERTEX_POINT ( 'NONE', #764 ) ;
#4181 = ADVANCED_FACE ( 'NONE', ( #12885 ), #5013, .T. ) ;
#4182 = CARTESIAN_POINT ( 'NONE',  ( 34.13493236988740165, 20.79694577678859702, 259.0935598591244684 ) ) ;
#4183 = EDGE_CURVE ( 'NONE', #167, #9614, #12947, .T. ) ;
#4184 = CARTESIAN_POINT ( 'NONE',  ( -245.1341653173766701, 8.810613775113198542, -8.147076446705556307 ) ) ;
#4185 = CARTESIAN_POINT ( 'NONE',  ( -197.8197553893909912, 19.00000000000000000, 58.77553482999130807 ) ) ;
#4186 = CARTESIAN_POINT ( 'NONE',  ( -242.3262939453856006, -6.637532586610901397, -9.695808798832128872 ) ) ;
#4187 = CARTESIAN_POINT ( 'NONE',  ( 239.5143764665039043, -1.545628037973273861, 3.140199927189666340 ) ) ;
#4188 = DIRECTION ( 'NONE',  ( 0.7823834078220596178, 0.5538822189107471816, 0.2847642722309944863 ) ) ;
#4189 = CARTESIAN_POINT ( 'NONE',  ( 240.5163796273739933, 3.187645493190168544, -1.494965077647770535 ) ) ;
#4190 = CONTEXT_DEPENDENT_SHAPE_REPRESENTATION ( #4499, #7935 ) ;
#4191 = AXIS2_PLACEMENT_3D ( 'NONE', #9357, #12483, #4537 ) ;
#4192 = DIRECTION ( 'NONE',  ( -0.000000000000000000, -1.000000000000000000, 0.000000000000000000 ) ) ;
#4193 = VERTEX_POINT ( 'NONE', #3749 ) ;
#4194 = ORIENTED_EDGE ( 'NONE', *, *, #1434, .T. ) ;
#4195 = CARTESIAN_POINT ( 'NONE',  ( -158.9353507255915190, 20.08915143292644245, -207.1687172315094756 ) ) ;
#4196 = EDGE_CURVE ( 'NONE', #11418, #6137, #3093, .T. ) ;
#4197 = DIRECTION ( 'NONE',  ( -0.000000000000000000, 1.000000000000000000, 0.000000000000000000 ) ) ;
#4198 = CARTESIAN_POINT ( 'NONE',  ( 239.3703217811417119, -1.345486616489417031, -3.231439195715531287 ) ) ;
#4199 = FACE_OUTER_BOUND ( 'NONE', #6439, .T. ) ;
#4200 = CARTESIAN_POINT ( 'NONE',  ( -248.8841473305942031, -9.947364712437689604, 6.711964937432249201 ) ) ;
#4201 = ADVANCED_FACE ( 'NONE', ( #3136 ), #4642, .F. ) ;
#4202 = CARTESIAN_POINT ( 'NONE',  ( 0.000000000000000000, -2.926905849962176352E-14, 0.000000000000000000 ) ) ;
#4203 = DIRECTION ( 'NONE',  ( 0.4226182617407092668, 0.000000000000000000, -0.9063077870366453848 ) ) ;
#4204 = CYLINDRICAL_SURFACE ( 'NONE', #3927, 5.500000000000005329 ) ;
#4205 = ITEM_DEFINED_TRANSFORMATION ( 'NONE', 'NONE', #3796,  #805 ) ;
#4206 = AXIS2_PLACEMENT_3D ( 'NONE', #3145, #8237, #35 ) ;
#4207 = EDGE_LOOP ( 'NONE', ( #12770, #7622, #4983, #6830 ) ) ;
#4208 = CARTESIAN_POINT ( 'NONE',  ( 240.4516407507180134, -2.994726891292637028, -1.822055168134961489 ) ) ;
#4209 = CARTESIAN_POINT ( 'NONE',  ( 229.9831997411649525, -2.134968791774042529, -2.782786951242176787 ) ) ;
#4210 = VERTEX_POINT ( 'NONE', #4147 ) ;
#4211 = ORIENTED_EDGE ( 'NONE', *, *, #10605, .F. ) ;
#4212 = DIRECTION ( 'NONE',  ( -0.4503334343941575724, 0.7071067811865460184, -0.5451603414287993221 ) ) ;
#4213 = CARTESIAN_POINT ( 'NONE',  ( -122.2593324768321992, 29.00000000000000000, 162.7755348299905052 ) ) ;
#4214 = AXIS2_PLACEMENT_3D ( 'NONE', #8151, #5006, #12345 ) ;
#4215 = CARTESIAN_POINT ( 'NONE',  ( 67.76049180280260487, 20.55460285165543155, -252.9796497734500917 ) ) ;
#4216 = DIRECTION ( 'NONE',  ( -0.000000000000000000, -1.000000000000000000, 0.000000000000000000 ) ) ;
#4217 = DIRECTION ( 'NONE',  ( -0.1736481776669307198, 0.000000000000000000, 0.9848077530122080203 ) ) ;
#4218 = CARTESIAN_POINT ( 'NONE',  ( -243.4706526635933983, 7.711678326568429220, 8.866250685001064724 ) ) ;
#4219 = ORIENTED_EDGE ( 'NONE', *, *, #3940, .F. ) ;
#4220 = AXIS2_PLACEMENT_3D ( 'NONE', #1088, #160, #7227 ) ;
#4221 = AXIS2_PLACEMENT_3D ( 'NONE', #4177, #7182, #185 ) ;
#4222 = CARTESIAN_POINT ( 'NONE',  ( 178.3611219674583310, 20.79694577634646535, 190.4297758776779403 ) ) ;
#4223 = CIRCLE ( 'NONE', #9974, 5.500000000000005329 ) ;
#4225 = ORIENTED_EDGE ( 'NONE', *, *, #519, .F. ) ;
#4224 = AXIS2_PLACEMENT_3D ( 'NONE', #10925, #7997, #12057 ) ;
#4226 = AXIS2_PLACEMENT_3D ( 'NONE', #25, #1082, #7156 ) ;
#4227 = LINE ( 'NONE', #5364, #7567 ) ;
#4228 = ORIENTED_EDGE ( 'NONE', *, *, #9934, .F. ) ;
#4229 = VERTEX_POINT ( 'NONE', #8229 ) ;
#4230 = CIRCLE ( 'NONE', #4019, 250.1999999999999602 ) ;
#4231 = EDGE_CURVE ( 'NONE', #10245, #10624, #9131, .T. ) ;
#4232 = CARTESIAN_POINT ( 'NONE',  ( 240.3826708216974737, 2.772967769358989809, 2.135567781667440102 ) ) ;
#4233 = DIRECTION ( 'NONE',  ( 0.000000000000000000, 0.000000000000000000, -1.000000000000000000 ) ) ;
#4234 = CARTESIAN_POINT ( 'NONE',  ( -0.000000000000000000, -30.00000000000000000, 0.000000000000000000 ) ) ;
#4235 = CARTESIAN_POINT ( 'NONE',  ( -122.2593324768359935, 18.00000000000000000, -168.2755348299880040 ) ) ;
#4236 = VECTOR ( 'NONE', #12584, 1000.000000000000114 ) ;
#4237 = CARTESIAN_POINT ( 'NONE',  ( -137.6665579279351448, 20.08915143297737060, -221.3800702329289720 ) ) ;
#4238 = FILL_AREA_STYLE ('',( #9310 ) ) ;
#4239 = VECTOR ( 'NONE', #2019, 1000.000000000000000 ) ;
#4240 = CONTEXT_DEPENDENT_SHAPE_REPRESENTATION ( #6175, #8922 ) ;
#4241 = ORIENTED_EDGE ( 'NONE', *, *, #10221, .T. ) ;
#4242 = DIRECTION ( 'NONE',  ( 0.000000000000000000, 1.000000000000000000, 0.000000000000000000 ) ) ;
#4243 = ORIENTED_EDGE ( 'NONE', *, *, #10480, .T. ) ;
#4244 = CARTESIAN_POINT ( 'NONE',  ( 2.816687638038912194E-14, -19.00000000000000000, 230.0000000000000000 ) ) ;
#4245 = CARTESIAN_POINT ( 'NONE',  ( -243.4720072945285096, -7.721209753983143464, -9.186020676454910827 ) ) ;
#4246 = CIRCLE ( 'NONE', #5087, 5.500000000000005329 ) ;
#4247 = CARTESIAN_POINT ( 'NONE',  ( -249.7885090780623614, -11.63841214936962309, 1.617571278916385191 ) ) ;
#4248 = EDGE_LOOP ( 'NONE', ( #787, #12563, #12783, #11818 ) ) ;
#4249 = EDGE_CURVE ( 'NONE', #6601, #4565, #11285, .T. ) ;
#4250 = CARTESIAN_POINT ( 'NONE',  ( -67.61424743051179576, 20.79694577629433283, 252.4341100433384781 ) ) ;
#4251 = CARTESIAN_POINT ( 'NONE',  ( -244.7207088138438280, 8.581273372657582499, -8.388577724893742982 ) ) ;
#4252 = CARTESIAN_POINT ( 'NONE',  ( 159.3442861576696714, -11.79660968244695951, 192.8974817588417068 ) ) ;
#4253 = CARTESIAN_POINT ( 'NONE',  ( -245.6948533279551157, -9.079155725198473803, -7.458842555897192028 ) ) ;
#4254 = AXIS2_PLACEMENT_3D ( 'NONE', #11544, #540, #4394 ) ;
#4255 = CARTESIAN_POINT ( 'NONE',  ( 239.7229759534581888, -1.780302303530038266, 3.014465403709621683 ) ) ;
#4256 = PRODUCT_DEFINITION_SHAPE ( 'NONE', 'NONE',  #13067 ) ;
#4257 = EDGE_CURVE ( 'NONE', #7755, #158, #9943, .T. ) ;
#4258 = CARTESIAN_POINT ( 'NONE',  ( 160.3845033201290846, -9.830508068730530624, 194.1567379013694392 ) ) ;
#4259 = EDGE_CURVE ( 'NONE', #1020, #4577, #4016, .T. ) ;
#4260 = DIRECTION ( 'NONE',  ( 1.000000000000000000, 0.000000000000000000, 0.000000000000000000 ) ) ;
#4261 = ORIENTED_EDGE ( 'NONE', *, *, #5542, .T. ) ;
#4262 = CARTESIAN_POINT ( 'NONE',  ( -67.71318189681706201, 19.96883746180772690, 252.8031682256479655 ) ) ;
#4263 = CARTESIAN_POINT ( 'NONE',  ( 0.000000000000000000, -19.00000000000000000, 0.000000000000000000 ) ) ;
#4264 = CARTESIAN_POINT ( 'NONE',  ( 23.54981712579821362, -30.00000000000000000, -295.6955080056602583 ) ) ;
#4265 = CARTESIAN_POINT ( 'NONE',  ( -122.2593324768359935, 18.00000000000000000, -168.2755348299880040 ) ) ;
#4266 = AXIS2_PLACEMENT_3D ( 'NONE', #2714, #6678, #8735 ) ;
#4267 = DIRECTION ( 'NONE',  ( 0.000000000000000000, 1.000000000000000000, 0.000000000000000000 ) ) ;
#4268 = CARTESIAN_POINT ( 'NONE',  ( -247.4131856421704470, -9.690266168923910683, 7.079595845687837397 ) ) ;
#4269 = CARTESIAN_POINT ( 'NONE',  ( 0.000000000000000000, -2.957522019940860139E-14, 0.000000000000000000 ) ) ;
#4270 = CARTESIAN_POINT ( 'NONE',  ( -7.267391899530093902, -138.4705547276867321, 41.21542755584194850 ) ) ;
#4271 = EDGE_CURVE ( 'NONE', #12676, #468, #10829, .T. ) ;
#4272 = CARTESIAN_POINT ( 'NONE',  ( -245.8522126016038101, -9.151584521558959295, 7.371153476891942447 ) ) ;
#4273 = EDGE_CURVE ( 'NONE', #11841, #1954, #5292, .T. ) ;
#4274 = VERTEX_POINT ( 'NONE', #4343 ) ;
#4275 = DIRECTION ( 'NONE',  ( 0.000000000000000000, 1.000000000000000000, 0.000000000000000000 ) ) ;
#4276 = DIRECTION ( 'NONE',  ( -0.000000000000000000, -1.000000000000000000, 0.000000000000000000 ) ) ;
#4277 = DIRECTION ( 'NONE',  ( 0.6368676505102716101, 0.000000000000000000, 0.7709731485165527420 ) ) ;
#4278 = EDGE_LOOP ( 'NONE', ( #6101, #8536 ) ) ;
#4279 = EDGE_LOOP ( 'NONE', ( #6552, #3884, #4097, #5555 ) ) ;
#4280 = ADVANCED_FACE ( 'NONE', ( #9216 ), #220, .F. ) ;
#4281 = DIRECTION ( 'NONE',  ( 0.000000000000000000, 1.000000000000000000, 0.000000000000000000 ) ) ;
#4282 = DIRECTION ( 'NONE',  ( -0.000000000000000000, -1.000000000000000000, 0.000000000000000000 ) ) ;
#4283 = CARTESIAN_POINT ( 'NONE',  ( -226.7975291067479588, 20.55460285112940610, -130.9697226053176564 ) ) ;
#4284 = AXIS2_PLACEMENT_3D ( 'NONE', #844, #6917, #1975 ) ;
#4285 = CARTESIAN_POINT ( 'NONE',  ( 84.02568524192950861, 20.79694577611522632, 247.4557548104415048 ) ) ;
#4286 = DIRECTION ( 'NONE',  ( 1.000000000000000000, 0.000000000000000000, 0.000000000000000000 ) ) ;
#4287 = CARTESIAN_POINT ( 'NONE',  ( -240.6618454235808997, 4.173161342497821558, 10.98396364135080461 ) ) ;
#4288 = EDGE_CURVE ( 'NONE', #5643, #8360, #2078, .T. ) ;
#4289 = ORIENTED_EDGE ( 'NONE', *, *, #10186, .F. ) ;
#4290 = DIRECTION ( 'NONE',  ( 0.000000000000000000, 0.000000000000000000, -1.000000000000000000 ) ) ;
#4291 = ORIENTED_EDGE ( 'NONE', *, *, #5991, .T. ) ;
#4292 = DIRECTION ( 'NONE',  ( -0.000000000000000000, -1.000000000000000000, 0.000000000000000000 ) ) ;
#4293 = ORIENTED_EDGE ( 'NONE', *, *, #3915, .T. ) ;
#4294 = ORIENTED_EDGE ( 'NONE', *, *, #4821, .T. ) ;
#4295 = DIRECTION ( 'NONE',  ( -0.000000000000000000, -1.000000000000000000, 0.000000000000000000 ) ) ;
#4296 = DIRECTION ( 'NONE',  ( 0.000000000000000000, 0.000000000000000000, 1.000000000000000000 ) ) ;
#4297 = DIRECTION ( 'NONE',  ( 0.6368676505102716101, 0.000000000000000000, 0.7709731485165527420 ) ) ;
#4298 = DIRECTION ( 'NONE',  ( 1.000000000000000000, 1.224646799147352961E-16, 0.000000000000000000 ) ) ;
#4299 = LINE ( 'NONE', #6904, #945 ) ;
#4300 = CARTESIAN_POINT ( 'NONE',  ( -244.4094253640295449, 8.392574418407512837, 8.577616032622085385 ) ) ;
#4301 = DIRECTION ( 'NONE',  ( 0.000000000000000000, -0.01970892327970899874, -0.9998057603070481525 ) ) ;
#4302 = CIRCLE ( 'NONE', #2390, 3.350000000000000089 ) ;
#4303 = CONTEXT_DEPENDENT_SHAPE_REPRESENTATION ( #9568, #4872 ) ;
#4304 = ORIENTED_EDGE ( 'NONE', *, *, #11690, .T. ) ;
#4305 = CARTESIAN_POINT ( 'NONE',  ( -194.2446334056326123, -19.00000000000000000, -235.1468102975487682 ) ) ;
#4306 = AXIS2_PLACEMENT_3D ( 'NONE', #757, #685, #619 ) ;
#4307 = VERTEX_POINT ( 'NONE', #2346 ) ;
#4308 = AXIS2_PLACEMENT_3D ( 'NONE', #9013, #10074, #9140 ) ;
#4309 = FACE_OUTER_BOUND ( 'NONE', #3537, .T. ) ;
#4310 = CARTESIAN_POINT ( 'NONE',  ( -160.3845033201972115, 9.830508068689120194, -194.1567379014518906 ) ) ;
#4311 = CARTESIAN_POINT ( 'NONE',  ( 197.8197553893915028, 29.00000000000000000, -64.27553482998990830 ) ) ;
#4312 = EDGE_LOOP ( 'NONE', ( #6192, #2582, #13020, #5363 ) ) ;
#4313 = DIRECTION ( 'NONE',  ( 0.000000000000000000, 0.000000000000000000, -1.000000000000000000 ) ) ;
#4314 = DIRECTION ( 'NONE',  ( 0.000000000000000000, 0.000000000000000000, 1.000000000000000000 ) ) ;
#4315 = CARTESIAN_POINT ( 'NONE',  ( -239.4459774607273346, 1.775548040146878614, 11.86792666930613116 ) ) ;
#4316 = AXIS2_PLACEMENT_3D ( 'NONE', #2729, #6820, #7615 ) ;
#4317 = CARTESIAN_POINT ( 'NONE',  ( -229.9691448513986529, 11.13025846491926885, 3.785357242864812122 ) ) ;
#4318 = CARTESIAN_POINT ( 'NONE',  ( 239.0530249120693327, -0.6193663072279376181, 3.444815813525719861 ) ) ;
#4319 = DIRECTION ( 'NONE',  ( 0.9063077870366552657, 0.000000000000000000, -0.4226182617406878950 ) ) ;
#4320 = EDGE_CURVE ( 'NONE', #2539, #11730, #3872, .T. ) ;
#4321 = CARTESIAN_POINT ( 'NONE',  ( -229.7549662686524243, 5.608571857102900182, -10.61518803634819008 ) ) ;
#4322 = EDGE_CURVE ( 'NONE', #1020, #4307, #3600, .T. ) ;
#4323 = CIRCLE ( 'NONE', #9639, 5.500000000000005329 ) ;
#4324 = AXIS2_PLACEMENT_3D ( 'NONE', #8321, #12380, #2244 ) ;
#4325 = DIRECTION ( 'NONE',  ( 0.000000000000000000, 1.000000000000000000, 0.000000000000000000 ) ) ;
#4326 = ORIENTED_EDGE ( 'NONE', *, *, #10291, .F. ) ;
#4327 = CARTESIAN_POINT ( 'NONE',  ( 130.5770120874479971, 20.08915143273683412, 226.1171533175384809 ) ) ;
#4328 = DIRECTION ( 'NONE',  ( 0.000000000000000000, 1.000000000000000000, 0.000000000000000000 ) ) ;
#4329 = CYLINDRICAL_SURFACE ( 'NONE', #1040, 239.0000000000000000 ) ;
#4330 = CARTESIAN_POINT ( 'NONE',  ( -249.2664547940201203, 10.49941023132624807, 5.274932156596537247 ) ) ;
#4331 = CARTESIAN_POINT ( 'NONE',  ( 0.000000000000000000, 0.000000000000000000, 0.000000000000000000 ) ) ;
#4332 = CARTESIAN_POINT ( 'NONE',  ( -0.000000000000000000, -2.772967769358684720, 0.000000000000000000 ) ) ;
#4333 = CARTESIAN_POINT ( 'NONE',  ( -246.3021867260266333, -9.336273485124390703, 7.538834026449642067 ) ) ;
#4334 = AXIS2_PLACEMENT_3D ( 'NONE', #1491, #10685, #9494 ) ;
#4335 = CARTESIAN_POINT ( 'NONE',  ( 197.8197553893915028, 30.00000000000000000, -64.27553482998990830 ) ) ;
#4336 = CARTESIAN_POINT ( 'NONE',  ( -24.00488622054087173, -138.4705547276867321, 34.28253040793660489 ) ) ;
#4337 = CIRCLE ( 'NONE', #9459, 10.00000000000000178 ) ;
#4338 = DIRECTION ( 'NONE',  ( 0.000000000000000000, 0.000000000000000000, 1.000000000000000000 ) ) ;
#4339 = ITEM_DEFINED_TRANSFORMATION ( 'NONE', 'NONE', #10176,  #805 ) ;
#4340 = SHAPE_REPRESENTATION ( 'Drain Plug', ( #805 ), #1657 ) ;
#4341 = ORIENTED_EDGE ( 'NONE', *, *, #8399, .F. ) ;
#4342 = CARTESIAN_POINT ( 'NONE',  ( 240.5832516929892222, -3.370511182595831379, 0.9484507947687070839 ) ) ;
#4343 = CARTESIAN_POINT ( 'NONE',  ( 189.4681260268079086, -19.00000000000000000, 229.3645116836727311 ) ) ;
#4344 = VERTEX_POINT ( 'NONE', #8549 ) ;
#4345 = ORIENTED_EDGE ( 'NONE', *, *, #6118, .T. ) ;
#4346 = CONICAL_SURFACE ( 'NONE', #8822, 6.500000000000005329, 0.7853981633974547183 ) ;
#4347 = DIRECTION ( 'NONE',  ( 0.000000000000000000, 0.000000000000000000, 1.000000000000000000 ) ) ;
#4348 = DIRECTION ( 'NONE',  ( 0.000000000000000000, 1.000000000000000000, 0.000000000000000000 ) ) ;
#4349 = EDGE_CURVE ( 'NONE', #3851, #4889, #479, .T. ) ;
#4350 = B_SPLINE_CURVE_WITH_KNOTS ( 'NONE', 3,
 ( #11534, #139, #5326, #4386, #2193, #6272, #12523, #199, #11331, #3379, #10323, #7194, #1202, #5259, #336, #4189, #6334, #8467 ),
 .UNSPECIFIED., .F., .F.,
 ( 4, 2, 2, 2, 2, 2, 2, 2, 4 ),
 ( 0.000000000000000000, 0.1250000000000028588, 0.1875000000000042744, 0.2500000000000057176, 0.5000000000000069944, 0.6250000000000076605, 0.6875000000000074385, 0.7500000000000071054, 1.000000000000000000 ),
 .UNSPECIFIED. ) ;
#4351 = EDGE_CURVE ( 'NONE', #9382, #4180, #11332, .T. ) ;
#4352 = CARTESIAN_POINT ( 'NONE',  ( 252.8031682264636117, 19.96883746172993668, -67.71318189737802129 ) ) ;
#4353 = CARTESIAN_POINT ( 'NONE',  ( 122.2593324768334071, 30.00000000000000000, -168.2755348299895104 ) ) ;
#4354 = DIRECTION ( 'NONE',  ( 0.4999999999999980016, 0.000000000000000000, 0.8660254037844398178 ) ) ;
#4355 = CARTESIAN_POINT ( 'NONE',  ( 71.82423009839129691, 19.40000000000000213, 192.2354503650404922 ) ) ;
#4356 = CARTESIAN_POINT ( 'NONE',  ( -260.3553053170167004, 20.79694577634646535, -17.06764083276478772 ) ) ;
#4357 = AXIS2_PLACEMENT_3D ( 'NONE', #9929, #8003, #13000 ) ;
#4358 = ORIENTED_EDGE ( 'NONE', *, *, #6319, .T. ) ;
#4359 = CARTESIAN_POINT ( 'NONE',  ( 252.0229195836992062, 20.79694577634646535, 67.53249125288881771 ) ) ;
#4360 = ORIENTED_EDGE ( 'NONE', *, *, #11711, .T. ) ;
#4361 = CARTESIAN_POINT ( 'NONE',  ( 220.3999999999999773, -2.249562960690858038, 0.04434507737934551691 ) ) ;
#4362 = ORIENTED_EDGE ( 'NONE', *, *, #6458, .F. ) ;
#4363 = ORIENTED_EDGE ( 'NONE', *, *, #10793, .T. ) ;
#4364 = CARTESIAN_POINT ( 'NONE',  ( 197.8197553893915028, 30.00000000000000000, -64.27553482998990830 ) ) ;
#4365 = EDGE_CURVE ( 'NONE', #8176, #6169, #11680, .T. ) ;
#4366 = CARTESIAN_POINT ( 'NONE',  ( 0.000000000000000000, 19.00000000000000000, -208.0000000000000000 ) ) ;
#4367 = DIRECTION ( 'NONE',  ( 1.000000000000000000, 0.000000000000000000, 0.000000000000000000 ) ) ;
#4368 = CARTESIAN_POINT ( 'NONE',  ( 239.1625895582377552, 0.9513411440000743013, -3.369326940753043953 ) ) ;
#4369 = DIRECTION ( 'NONE',  ( -1.000000000000000000, 0.000000000000000000, 0.000000000000000000 ) ) ;
#4370 = CARTESIAN_POINT ( 'NONE',  ( -246.1949466625434866, 9.295128601630475274, 7.589564689875960113 ) ) ;
#4371 = EDGE_CURVE ( 'NONE', #6121, #1707, #6658, .T. ) ;
#4372 = ORIENTED_EDGE ( 'NONE', *, *, #3287, .T. ) ;
#4373 = DIRECTION ( 'NONE',  ( 0.000000000000000000, -1.000000000000000000, 0.000000000000000000 ) ) ;
#4374 = CIRCLE ( 'NONE', #7359, 249.7999999999999829 ) ;
#4375 = ORIENTED_EDGE ( 'NONE', *, *, #4966, .T. ) ;
#4376 =( REPRESENTATION_RELATIONSHIP ('NONE','NONE', #12019, #182 ) REPRESENTATION_RELATIONSHIP_WITH_TRANSFORMATION ( #11725 )SHAPE_REPRESENTATION_RELATIONSHIP( ) );
#4377 = DIRECTION ( 'NONE',  ( 0.000000000000000000, -1.000000000000000000, 0.000000000000000000 ) ) ;
#4378 = CARTESIAN_POINT ( 'NONE',  ( 227.3999999999999773, 0.000000000000000000, 0.000000000000000000 ) ) ;
#4379 = CARTESIAN_POINT ( 'NONE',  ( 137.6665579279354006, 20.08915143297737060, -221.3800702329289152 ) ) ;
#4380 = EDGE_LOOP ( 'NONE', ( #5976, #6224, #4981, #10289 ) ) ;
#4381 = DIRECTION ( 'NONE',  ( 0.000000000000000000, 0.000000000000000000, -1.000000000000000000 ) ) ;
#4382 = CARTESIAN_POINT ( 'NONE',  ( -243.5834864928935417, 7.809424032089159695, -9.110990436254303049 ) ) ;
#4383 = CARTESIAN_POINT ( 'NONE',  ( 238.9743710159888224, -9.335707311080796797E-14, -3.499999942258349428 ) ) ;
#4384 = CARTESIAN_POINT ( 'NONE',  ( -229.9419135018622171, 10.55618113774804101, 5.217406956883983149 ) ) ;
#4385 = DIRECTION ( 'NONE',  ( 0.9659258262890717539, 0.000000000000000000, -0.2588190451025078609 ) ) ;
#4386 = CARTESIAN_POINT ( 'NONE',  ( 240.4969650423413725, 3.129188642588045077, 1.571450734147935790 ) ) ;
#4387 = DIRECTION ( 'NONE',  ( 0.000000000000000000, 1.000000000000000000, 0.000000000000000000 ) ) ;
#4388 = ORIENTED_EDGE ( 'NONE', *, *, #8609, .F. ) ;
#4389 = CARTESIAN_POINT ( 'NONE',  ( 172.5787240287708073, 19.96883745935533838, 196.7513681801829932 ) ) ;
#4390 = DIRECTION ( 'NONE',  ( 0.000000000000000000, 1.000000000000000000, 0.000000000000000000 ) ) ;
#4391 = DIRECTION ( 'NONE',  ( 0.6368676505102707219, 0.000000000000000000, 0.7709731485165535192 ) ) ;
#4392 = PRODUCT_DEFINITION_SHAPE ( 'NONE', 'NONE',  #13183 ) ;
#4393 = EDGE_CURVE ( 'NONE', #2888, #8825, #12867, .T. ) ;
#4394 = DIRECTION ( 'NONE',  ( 0.000000000000000000, 0.000000000000000000, -1.000000000000000000 ) ) ;
#4395 = DIRECTION ( 'NONE',  ( -0.6368676505102708330, 0.000000000000000000, -0.7709731485165536302 ) ) ;
#4396 = CARTESIAN_POINT ( 'NONE',  ( 235.4000000000000057, -2.749465840844381948, 0.05419953901920007699 ) ) ;
#4397 = CARTESIAN_POINT ( 'NONE',  ( -29.59329699131390257, -138.4705547276867321, 29.59329699131380309 ) ) ;
#4398 = CARTESIAN_POINT ( 'NONE',  ( 197.8197553893920144, 30.00000000000000000, 64.27553482998850143 ) ) ;
#4399 = CARTESIAN_POINT ( 'NONE',  ( -0.000000000000000000, -25.00000000000000000, 0.000000000000000000 ) ) ;
#4400 = CARTESIAN_POINT ( 'NONE',  ( 6.337788322448691496E-13, 20.79694577634647601, -260.7745447061711275 ) ) ;
#4401 = ORIENTED_EDGE ( 'NONE', *, *, #12873, .T. ) ;
#4402 = EDGE_LOOP ( 'NONE', ( #12692, #631, #41, #11347 ) ) ;
#4403 = DIRECTION ( 'NONE',  ( 0.000000000000000000, -1.000000000000000000, 0.000000000000000000 ) ) ;
#4404 = CARTESIAN_POINT ( 'NONE',  ( -159.6627199829249264, -22.00000000000000000, -193.2829683330999728 ) ) ;
#4405 = EDGE_CURVE ( 'NONE', #6551, #2184, #11118, .T. ) ;
#4406 = CARTESIAN_POINT ( 'NONE',  ( -172.6991790971032970, 20.55460285072942384, -196.8887528238318509 ) ) ;
#4407 = CIRCLE ( 'NONE', #381, 249.7999999999999829 ) ;
#4408 = CARTESIAN_POINT ( 'NONE',  ( 122.2593324768346008, 30.00000000000000000, 168.2755348299889988 ) ) ;
#4409 = CARTESIAN_POINT ( 'NONE',  ( 0.000000000000000000, 0.000000000000000000, 0.000000000000000000 ) ) ;
#4410 = DIRECTION ( 'NONE',  ( 0.000000000000000000, 1.000000000000000000, 0.000000000000000000 ) ) ;
#4411 = CARTESIAN_POINT ( 'NONE',  ( -260.7745447061711843, 20.79694577634646535, 8.533827019709271156 ) ) ;
#4412 = VERTEX_POINT ( 'NONE', #2408 ) ;
#4413 = CARTESIAN_POINT ( 'NONE',  ( 34.05310945291996916, 20.79694577634646535, -258.6823826759385270 ) ) ;
#4414 = ADVANCED_FACE ( 'NONE', ( #8482 ), #6550, .F. ) ;
#4415 = VERTEX_POINT ( 'NONE', #10739 ) ;
#4416 = EDGE_CURVE ( 'NONE', #9350, #12436, #6447, .T. ) ;
#4417 = DIRECTION ( 'NONE',  ( 0.000000000000000000, 0.8757116489157734662, 0.4828344519120573719 ) ) ;
#4418 = ORIENTED_EDGE ( 'NONE', *, *, #5760, .T. ) ;
#4419 = VERTEX_POINT ( 'NONE', #352 ) ;
#4420 = AXIS2_PLACEMENT_3D ( 'NONE', #2223, #6301, #10350 ) ;
#4421 = DIRECTION ( 'NONE',  ( 0.000000000000000000, 0.000000000000000000, -1.000000000000000000 ) ) ;
#4422 = DIRECTION ( 'NONE',  ( -0.6368676505102706109, 0.000000000000000000, -0.7709731485165535192 ) ) ;
#4423 = CARTESIAN_POINT ( 'NONE',  ( 197.8197553893915028, 19.00000000000000000, -58.77553482998990830 ) ) ;
#4424 = CARTESIAN_POINT ( 'NONE',  ( -239.5361044668155159, 1.848645179572584896, -11.60366368868220022 ) ) ;
#4425 = DIRECTION ( 'NONE',  ( -0.000000000000000000, -1.000000000000000000, 0.000000000000000000 ) ) ;
#4426 =( LENGTH_UNIT ( ) NAMED_UNIT ( * ) SI_UNIT ( .MILLI., .METRE. ) );
#4427 = AXIS2_PLACEMENT_3D ( 'NONE', #8487, #9483, #7674 ) ;
#4428 = AXIS2_PLACEMENT_3D ( 'NONE', #6278, #9469, #1335 ) ;
#4429 = AXIS2_PLACEMENT_3D ( 'NONE', #4409, #12743, #3407 ) ;
#4430 = ORIENTED_EDGE ( 'NONE', *, *, #11828, .T. ) ;
#4431 = CARTESIAN_POINT ( 'NONE',  ( 225.1241593668336236, -19.00000000000000000, -185.9653539489990521 ) ) ;
#4432 = ORIENTED_EDGE ( 'NONE', *, *, #6458, .T. ) ;
#4433 = EDGE_CURVE ( 'NONE', #4958, #12890, #4094, .T. ) ;
#4434 = CARTESIAN_POINT ( 'NONE',  ( 122.2593324768346008, 19.00000000000000000, 162.7755348299889988 ) ) ;
#4435 = CARTESIAN_POINT ( 'NONE',  ( -0.000000000000000000, -3.327561323230905366, 0.000000000000000000 ) ) ;
#4436 = CARTESIAN_POINT ( 'NONE',  ( 251.8100110699623144, 20.08915143297736705, -67.47543992452008865 ) ) ;
#4437 = EDGE_CURVE ( 'NONE', #12119, #1218, #5796, .T. ) ;
#4438 = CIRCLE ( 'NONE', #3161, 305.0000000000000000 ) ;
#4439 = CARTESIAN_POINT ( 'NONE',  ( 0.000000000000000000, 2.772967769359004908, 0.000000000000000000 ) ) ;
#4440 = CARTESIAN_POINT ( 'NONE',  ( -243.6755871756574550, 7.880721788829606389, -9.049489450626314380 ) ) ;
#4441 = LINE ( 'NONE', #8525, #3173 ) ;
#4442 = CARTESIAN_POINT ( 'NONE',  ( 0.000000000000000000, 20.00000000000000000, 0.000000000000000000 ) ) ;
#4443 = AXIS2_PLACEMENT_3D ( 'NONE', #9155, #3752, #8888 ) ;
#4444 = CIRCLE ( 'NONE', #9555, 6.500000000000000888 ) ;
#4445 = DIRECTION ( 'NONE',  ( 0.6368676505102716101, 0.000000000000000000, 0.7709731485165527420 ) ) ;
#4446 = APPLICATION_PROTOCOL_DEFINITION ( 'draft international standard', 'automotive_design', 1998, #10454 ) ;
#4447 = CARTESIAN_POINT ( 'NONE',  ( -229.8175486381514361, 7.757877409022798432, -9.162773420015767556 ) ) ;
#4448 = ITEM_DEFINED_TRANSFORMATION ( 'NONE', 'NONE', #2756,  #805 ) ;
#4449 = AXIS2_PLACEMENT_3D ( 'NONE', #9971, #9838, #6657 ) ;
#4450 = CARTESIAN_POINT ( 'NONE',  ( 0.000000000000000000, 29.00000000000000000, -249.7999999999999829 ) ) ;
#4451 = ORIENTED_EDGE ( 'NONE', *, *, #5588, .T. ) ;
#4452 = CARTESIAN_POINT ( 'NONE',  ( -234.7354397754233446, 19.96883745989621417, -115.7315435906453871 ) ) ;
#4453 = DIRECTION ( 'NONE',  ( -0.6368676505102698338, 0.000000000000000000, -0.7709731485165542964 ) ) ;
#4454 = DIRECTION ( 'NONE',  ( 8.659560562354816994E-17, 0.7071067811865570096, -0.7071067811865380248 ) ) ;
#4455 = DIRECTION ( 'NONE',  ( 0.000000000000000000, 0.000000000000000000, 1.000000000000000000 ) ) ;
#4456 = VECTOR ( 'NONE', #8316, 1000.000000000000114 ) ;
#4457 = CARTESIAN_POINT ( 'NONE',  ( -137.6665579279357701, 20.08915143297736705, 221.3800702329286310 ) ) ;
#4458 = VECTOR ( 'NONE', #7518, 999.9999999999998863 ) ;
#4459 = DIRECTION ( 'NONE',  ( 0.000000000000000000, 0.000000000000000000, 1.000000000000000000 ) ) ;
#4460 = DIRECTION ( 'NONE',  ( -0.8325950321581960800, 0.5538822189107472926, -2.906990017593840060E-15 ) ) ;
#4461 = CARTESIAN_POINT ( 'NONE',  ( 71.82423009839129691, 18.00000000000000000, 203.8354503650404581 ) ) ;
#4462 = CARTESIAN_POINT ( 'NONE',  ( 193.6077657551222444, -30.00000000000000000, 234.3758371490322929 ) ) ;
#4463 = EDGE_CURVE ( 'NONE', #2690, #11555, #10486, .T. ) ;
#4464 = PRODUCT ( 'External Heavy Duty Rotating Flange Ring', 'External Heavy Duty Rotating Flange Ring', '', ( #4511 ) ) ;
#4465 = DIRECTION ( 'NONE',  ( -0.000000000000000000, -1.000000000000000000, 0.000000000000000000 ) ) ;
#4466 = VERTEX_POINT ( 'NONE', #8943 ) ;
#4467 = ORIENTED_EDGE ( 'NONE', *, *, #9054, .T. ) ;
#4468 = AXIS2_PLACEMENT_3D ( 'NONE', #1999, #1062, #6997 ) ;
#4469 = LINE ( 'NONE', #11622, #2519 ) ;
#4470 = FACE_BOUND ( 'NONE', #4278, .T. ) ;
#4471 = CONICAL_SURFACE ( 'NONE', #8961, 6.500000000000005329, 0.7853981633974476129 ) ;
#4472 = CARTESIAN_POINT ( 'NONE',  ( -34.20858920445061102, 20.55460285115536934, 259.6535381498995321 ) ) ;
#4473 = CARTESIAN_POINT ( 'NONE',  ( 227.3999999999999773, 2.172755033604258923, -3.940702420120982374 ) ) ;
#4474 = CARTESIAN_POINT ( 'NONE',  ( 0.000000000000000000, 0.000000000000000000, 0.000000000000000000 ) ) ;
#4475 = DIRECTION ( 'NONE',  ( 0.000000000000000000, -0.7071067811865460184, -0.7071067811865489050 ) ) ;
#4476 = CARTESIAN_POINT ( 'NONE',  ( 227.3999999999999773, 2.326370887777457153, 3.852012265362291465 ) ) ;
#4477 = DIRECTION ( 'NONE',  ( 1.000000000000000000, 0.000000000000000000, -1.224646799147353207E-16 ) ) ;
#4478 = ORIENTED_EDGE ( 'NONE', *, *, #2570, .T. ) ;
#4479 = EDGE_CURVE ( 'NONE', #8155, #8360, #6016, .T. ) ;
#4480 = FACE_OUTER_BOUND ( 'NONE', #4848, .T. ) ;
#4481 = EDGE_CURVE ( 'NONE', #12785, #12119, #6812, .T. ) ;
#4482 = ORIENTED_EDGE ( 'NONE', *, *, #3491, .T. ) ;
#4483 = LINE ( 'NONE', #10623, #6371 ) ;
#4484 = ORIENTED_EDGE ( 'NONE', *, *, #4463, .F. ) ;
#4485 = ORIENTED_EDGE ( 'NONE', *, *, #7306, .T. ) ;
#4486 = LINE ( 'NONE', #11573, #2615 ) ;
#4487 = EDGE_CURVE ( 'NONE', #5558, #10691, #3308, .T. ) ;
#4488 = DIRECTION ( 'NONE',  ( 1.000000000000000000, 0.000000000000000000, 0.000000000000000000 ) ) ;
#4489 = ADVANCED_FACE ( 'NONE', ( #12009 ), #10054, .T. ) ;
#4490 = CARTESIAN_POINT ( 'NONE',  ( 239.2050160255438414, 1.043887935153559487, -3.340720568028653137 ) ) ;
#4491 = FACE_OUTER_BOUND ( 'NONE', #12271, .T. ) ;
#4492 =( NAMED_UNIT ( * ) SI_UNIT ( $, .STERADIAN. ) SOLID_ANGLE_UNIT ( ) );
#4493 = AXIS2_PLACEMENT_3D ( 'NONE', #1105, #1939, #4033 ) ;
#4494 = CONTEXT_DEPENDENT_SHAPE_REPRESENTATION ( #11374, #1285 ) ;
#4495 = ORIENTED_EDGE ( 'NONE', *, *, #7170, .F. ) ;
#4496 = CARTESIAN_POINT ( 'NONE',  ( -238.7109915808064500, 2.244475480116206709E-14, 11.74999999995203126 ) ) ;
#4497 = CARTESIAN_POINT ( 'NONE',  ( -286.5445428119863323, -30.00000000000000000, -22.67813138875635204 ) ) ;
#4498 = VERTEX_POINT ( 'NONE', #1871 ) ;
#4499 =( REPRESENTATION_RELATIONSHIP ('NONE','NONE', #12019, #5191 ) REPRESENTATION_RELATIONSHIP_WITH_TRANSFORMATION ( #141 )SHAPE_REPRESENTATION_RELATIONSHIP( ) );
#4500 = CARTESIAN_POINT ( 'NONE',  ( -0.000000000000000000, -1.848645179577135034, 0.000000000000000000 ) ) ;
#4501 = CARTESIAN_POINT ( 'NONE',  ( 132.6365829178909621, -30.00000000000000000, -260.1259780660157048 ) ) ;
#4502 = DIRECTION ( 'NONE',  ( 0.000000000000000000, 0.9998057603070481525, -0.01970892327970900221 ) ) ;
#4503 = CARTESIAN_POINT ( 'NONE',  ( 195.9813743529078920, -25.00000000000000000, -161.8917567597108018 ) ) ;
#4504 = CARTESIAN_POINT ( 'NONE',  ( -238.7054577249708132, 0.2141779464642266373, 11.99854502510401666 ) ) ;
#4505 = EDGE_CURVE ( 'NONE', #58, #4577, #6944, .T. ) ;
#4506 = AXIS2_PLACEMENT_3D ( 'NONE', #5056, #4905, #8339 ) ;
#4507 = CARTESIAN_POINT ( 'NONE',  ( -241.0949697665562041, -4.988078590052489325, -10.64105268538957283 ) ) ;
#4508 = EDGE_CURVE ( 'NONE', #13016, #5655, #5943, .T. ) ;
#4509 = AXIS2_PLACEMENT_3D ( 'NONE', #4540, #5681, #1751 ) ;
#4510 = FACE_OUTER_BOUND ( 'NONE', #1623, .T. ) ;
#4511 = PRODUCT_CONTEXT ( 'NONE', #914, 'mechanical' ) ;
#4512 = AXIS2_PLACEMENT_3D ( 'NONE', #4040, #1111, #9378 ) ;
#4513 = CARTESIAN_POINT ( 'NONE',  ( -189.4681260268063170, -19.00000000000000000, -229.3645116836740385 ) ) ;
#4514 = CARTESIAN_POINT ( 'NONE',  ( -122.2593324768359935, 30.00000000000000000, -174.7755348299880040 ) ) ;
#4515 = ORIENTED_EDGE ( 'NONE', *, *, #4918, .T. ) ;
#4516 = CARTESIAN_POINT ( 'NONE',  ( -252.8031682270700458, 19.96883746027420869, -67.71318189758747508 ) ) ;
#4517 = CARTESIAN_POINT ( 'NONE',  ( 0.000000000000000000, -20.69999999999999929, 0.000000000000000000 ) ) ;
#4518 = CARTESIAN_POINT ( 'NONE',  ( 159.6627199829248980, -22.00000000000000000, 193.2829683331000012 ) ) ;
#4519 = STYLED_ITEM ( 'NONE', ( #7047 ), #10352 ) ;
#4520 = DIRECTION ( 'NONE',  ( 0.000000000000000000, 1.000000000000000000, 0.000000000000000000 ) ) ;
#4521 = ADVANCED_FACE ( 'NONE', ( #9871 ), #5375, .F. ) ;
#4522 = CARTESIAN_POINT ( 'NONE',  ( -83.79436865282377767, 20.08915143297736705, 246.8597181602068531 ) ) ;
#4523 = CARTESIAN_POINT ( 'NONE',  ( 0.000000000000000000, -19.00000000000000000, 0.000000000000000000 ) ) ;
#4524 = DIRECTION ( 'NONE',  ( -0.7210484489137202191, 0.5538822189107471816, 0.4162975160790962637 ) ) ;
#4525 = AXIS2_PLACEMENT_3D ( 'NONE', #5533, #6743, #10663 ) ;
#4526 = VECTOR ( 'NONE', #8635, 1000.000000000000114 ) ;
#4527 = CARTESIAN_POINT ( 'NONE',  ( 229.9884417198156257, 2.638064155344324924, 2.311452626510129615 ) ) ;
#4528 = CIRCLE ( 'NONE', #3898, 6.499999999999999112 ) ;
#4529 = CIRCLE ( 'NONE', #4963, 2.500000000000025313 ) ;
#4530 = CLOSED_SHELL ( 'NONE', ( #8249, #8248, #7368, #5086, #3507, #10945, #4936, #4081, #6467, #5477, #10240, #2123, #6318, #7662, #6147, #6484, #4201, #10961, #8527, #5620, #5327, #8026, #1086, #6365, #10127, #3410, #5540, #8719, #7463, #11753, #8484, #11030, #7267, #9861, #276, #6771, #1255, #7630, #11613, #11130, #10515, #8032, #3704, #11494, #7218, #2294, #9504, #3987, #8909, #7934, #445, #702, #1494, #6296, #10387, #1398, #7621, #4158, #4688, #9550, #2708, #4813, #4489, #11973, #1154, #8883, #11278, #8348, #6163, #385, #2671, #4835, #9778, #11379, #11527, #11258, #9078, #7528, #12163, #11541, #1803, #8836, #5406, #8856, #10773, #9053, #10862, #1199, #9174, #11049, #1963, #11003, #3359, #1109, #1137, #1748, #6621, #12349, #7144, #1346, #2837, #7214, #66, #1652, #4091, #1228, #11797, #2973, #177, #11785, #418 ) ) ;
#4531 = CARTESIAN_POINT ( 'NONE',  ( 171.9542656377731191, 0.000000000000000000, 208.1627500994694628 ) ) ;
#4532 = CONICAL_SURFACE ( 'NONE', #10668, 5.099999999999993427, 0.7853981633974461696 ) ;
#4533 = DIRECTION ( 'NONE',  ( -0.000000000000000000, -1.000000000000000000, 0.000000000000000000 ) ) ;
#4534 = ORIENTED_EDGE ( 'NONE', *, *, #1723, .T. ) ;
#4535 = EDGE_LOOP ( 'NONE', ( #7071, #1299 ) ) ;
#4536 = DIRECTION ( 'NONE',  ( 0.000000000000000000, 0.000000000000000000, 1.000000000000000000 ) ) ;
#4537 = DIRECTION ( 'NONE',  ( -1.224646799147349509E-16, 0.000000000000000000, -1.000000000000000000 ) ) ;
#4538 = CONICAL_SURFACE ( 'NONE', #5407, 5.500000000000005329, 0.7853981633974461696 ) ;
#4539 = CARTESIAN_POINT ( 'NONE',  ( -196.4640694352650030, 20.79694577634417030, 172.3268284098779759 ) ) ;
#4540 = CARTESIAN_POINT ( 'NONE',  ( -290.6841825403030839, -30.00000000000000000, -27.68945685411394919 ) ) ;
#4541 =( REPRESENTATION_RELATIONSHIP ('NONE','NONE', #12019, #4340 ) REPRESENTATION_RELATIONSHIP_WITH_TRANSFORMATION ( #786 )SHAPE_REPRESENTATION_RELATIONSHIP( ) );
#4542 = DIRECTION ( 'NONE',  ( -0.4226182617407033271, 0.000000000000000000, 0.9063077870366481603 ) ) ;
#4543 = CARTESIAN_POINT ( 'NONE',  ( 0.000000000000000000, 21.50000000000000000, -249.7999999999999829 ) ) ;
#4544 = CARTESIAN_POINT ( 'NONE',  ( -237.6585102388689563, 20.79694577634646535, 107.6783259591022244 ) ) ;
#4545 = ORIENTED_EDGE ( 'NONE', *, *, #9622, .F. ) ;
#4546 = CARTESIAN_POINT ( 'NONE',  ( 244.1900186690937460, 20.79694577634646535, -91.90986972409935163 ) ) ;
#4547 = AXIS2_PLACEMENT_3D ( 'NONE', #6412, #7401, #8280 ) ;
#4548 = ORIENTED_EDGE ( 'NONE', *, *, #5095, .F. ) ;
#4549 = CARTESIAN_POINT ( 'NONE',  ( -197.8197553893909912, 29.00000000000000000, 64.27553482999130097 ) ) ;
#4550 = ORIENTED_EDGE ( 'NONE', *, *, #6226, .F. ) ;
#4551 = ORIENTED_EDGE ( 'NONE', *, *, #5016, .T. ) ;
#4552 = DIRECTION ( 'NONE',  ( 1.000000000000000000, 0.000000000000000000, 0.000000000000000000 ) ) ;
#4553 = CARTESIAN_POINT ( 'NONE',  ( 3.061616997868383121E-14, 0.000000000000000000, 250.0000000000000000 ) ) ;
#4554 = EDGE_CURVE ( 'NONE', #11136, #5893, #12818, .T. ) ;
#4555 = ADVANCED_FACE ( 'NONE', ( #1065 ), #10190, .T. ) ;
#4556 = CARTESIAN_POINT ( 'NONE',  ( 239.5494890110568065, 1.589230970485129735, -3.118420702611433892 ) ) ;
#4557 = AXIS2_PLACEMENT_3D ( 'NONE', #9691, #1837, #8694 ) ;
#4558 = AXIS2_PLACEMENT_3D ( 'NONE', #12347, #7404, #11477 ) ;
#4559 = DIRECTION ( 'NONE',  ( 0.6368676505102716101, 0.000000000000000000, 0.7709731485165527420 ) ) ;
#4560 =( LENGTH_UNIT ( ) NAMED_UNIT ( * ) SI_UNIT ( .MILLI., .METRE. ) );
#4561 = DIRECTION ( 'NONE',  ( 0.000000000000000000, 0.000000000000000000, 1.000000000000000000 ) ) ;
#4562 = CONTEXT_DEPENDENT_SHAPE_REPRESENTATION ( #2018, #10364 ) ;
#4563 = VERTEX_POINT ( 'NONE', #8069 ) ;
#4564 = DIRECTION ( 'NONE',  ( -0.6368676505102696117, 0.000000000000000000, -0.7709731485165545184 ) ) ;
#4565 = VERTEX_POINT ( 'NONE', #12206 ) ;
#4566 = CARTESIAN_POINT ( 'NONE',  ( -243.8540711624768846, 8.004651165874994589, -8.601279203521002614 ) ) ;
#4567 = COLOUR_RGB ( '', 0.40784314, 0.44705882, 0.49803922) ;
#4568 = DIRECTION ( 'NONE',  ( 0.000000000000000000, 0.000000000000000000, -1.000000000000000000 ) ) ;
#4569 = CARTESIAN_POINT ( 'NONE',  ( -239.4297296705752558, 1.759293724106229861, 11.87033638227847909 ) ) ;
#4570 = CYLINDRICAL_SURFACE ( 'NONE', #2910, 5.099999999999993427 ) ;
#4571 = DIRECTION ( 'NONE',  ( 1.000000000000000000, 0.000000000000000000, 0.000000000000000000 ) ) ;
#4572 = CIRCLE ( 'NONE', #6088, 259.6078431372534396 ) ;
#4573 = DIRECTION ( 'NONE',  ( 0.000000000000000000, -1.000000000000000000, 0.000000000000000000 ) ) ;
#4574 = CONTEXT_DEPENDENT_SHAPE_REPRESENTATION ( #4541, #5211 ) ;
#4575 = CIRCLE ( 'NONE', #6729, 230.0000000000000000 ) ;
#4576 = CARTESIAN_POINT ( 'NONE',  ( -229.9447701116965277, 10.89162700641532666, 5.050967065786899468 ) ) ;
#4577 = VERTEX_POINT ( 'NONE', #10128 ) ;
#4578 = ADVANCED_FACE ( 'NONE', ( #6336 ), #7070, .F. ) ;
#4579 = ORIENTED_EDGE ( 'NONE', *, *, #9910, .F. ) ;
#4580 = ADVANCED_FACE ( 'NONE', ( #3058 ), #6275, .F. ) ;
#4581 = DIRECTION ( 'NONE',  ( 0.6368676505102709440, 0.000000000000000000, 0.7709731485165532971 ) ) ;
#4582 = ORIENTED_EDGE ( 'NONE', *, *, #10724, .F. ) ;
#4583 = CIRCLE ( 'NONE', #12047, 5.100000000000003197 ) ;
#4584 = CARTESIAN_POINT ( 'NONE',  ( 196.7513681799458709, 19.96883746115198122, -172.5787240287706936 ) ) ;
#4585 = DIRECTION ( 'NONE',  ( 0.000000000000000000, 1.000000000000000000, 0.000000000000000000 ) ) ;
#4586 = DIRECTION ( 'NONE',  ( 0.000000000000000000, 1.000000000000000000, 0.000000000000000000 ) ) ;
#4587 = DIRECTION ( 'NONE',  ( 1.000000000000000000, 0.000000000000000000, 0.000000000000000000 ) ) ;
#4588 = CARTESIAN_POINT ( 'NONE',  ( -240.0943994960961447, -2.684989249076883855, 11.43947242957905353 ) ) ;
#4589 = LINE ( 'NONE', #9661, #9637 ) ;
#4590 = DIRECTION ( 'NONE',  ( -0.6820219226572461491, 0.5538822189107472926, 0.4775568914688813060 ) ) ;
#4591 = CARTESIAN_POINT ( 'NONE',  ( 229.9901642561758592, 2.782416201478342455, -2.135548222472730462 ) ) ;
#4592 = CONTEXT_DEPENDENT_SHAPE_REPRESENTATION ( #10360, #11234 ) ;
#4593 = DIRECTION ( 'NONE',  ( 0.000000000000000000, 1.000000000000000000, 0.000000000000000000 ) ) ;
#4594 = EDGE_CURVE ( 'NONE', #11853, #4811, #9198, .T. ) ;
#4595 = DIRECTION ( 'NONE',  ( 0.000000000000000000, -1.000000000000000000, 0.000000000000000000 ) ) ;
#4596 = ORIENTED_EDGE ( 'NONE', *, *, #4083, .F. ) ;
#4597 = VERTEX_POINT ( 'NONE', #10389 ) ;
#4598 = CARTESIAN_POINT ( 'NONE',  ( 197.8197553893915028, 30.00000000000000000, -57.77553482998990830 ) ) ;
#4599 = DIRECTION ( 'NONE',  ( 0.6368676505102707219, 0.000000000000000000, 0.7709731485165535192 ) ) ;
#4600 = EDGE_CURVE ( 'NONE', #6169, #12610, #4938, .T. ) ;
#4601 = CARTESIAN_POINT ( 'NONE',  ( 261.3381329044966606, 20.55460285106647689, -17.10461161501038063 ) ) ;
#4602 = CARTESIAN_POINT ( 'NONE',  ( -161.8917567597108587, -22.00000000000000000, -195.9813743529078636 ) ) ;
#4603 = PRODUCT_DEFINITION_SHAPE ( 'NONE', 'NONE',  #13164 ) ;
#4604 = DIRECTION ( 'NONE',  ( -0.08715574274766177409, 0.000000000000000000, 0.9961946980917452121 ) ) ;
#4605 = DIRECTION ( 'NONE',  ( 0.000000000000000000, 1.000000000000000000, 0.000000000000000000 ) ) ;
#4606 = FACE_OUTER_BOUND ( 'NONE', #11737, .T. ) ;
#4607 = ORIENTED_EDGE ( 'NONE', *, *, #11867, .T. ) ;
#4608 = CARTESIAN_POINT ( 'NONE',  ( 237.6585102388688426, 20.79694577634646890, -107.6783259591024802 ) ) ;
#4609 = ORIENTED_EDGE ( 'NONE', *, *, #9485, .F. ) ;
#4610 = CARTESIAN_POINT ( 'NONE',  ( -171.9542656377731475, 19.00000000000000000, -208.1627500994694344 ) ) ;
#4611 = ORIENTED_EDGE ( 'NONE', *, *, #3382, .F. ) ;
#4612 = ORIENTED_EDGE ( 'NONE', *, *, #12838, .T. ) ;
#4613 = VERTEX_POINT ( 'NONE', #5121 ) ;
#4614 = DIRECTION ( 'NONE',  ( 0.000000000000000000, 1.000000000000000000, 0.000000000000000000 ) ) ;
#4615 = DIRECTION ( 'NONE',  ( -0.000000000000000000, -1.000000000000000000, 0.000000000000000000 ) ) ;
#4616 = CARTESIAN_POINT ( 'NONE',  ( 34.10614053577565130, 20.08915143319461905, -258.8746690710824510 ) ) ;
#4617 = DIRECTION ( 'NONE',  ( 0.000000000000000000, -1.000000000000000000, 0.000000000000000000 ) ) ;
#4618 = CARTESIAN_POINT ( 'NONE',  ( -290.6841825403030839, -29.00000000000000000, -27.68945685411394919 ) ) ;
#4619 = DIRECTION ( 'NONE',  ( -1.000000000000000000, 0.000000000000000000, 0.000000000000000000 ) ) ;
#4620 = ITEM_DEFINED_TRANSFORMATION ( 'NONE', 'NONE', #2717,  #805 ) ;
#4621 = ORIENTED_EDGE ( 'NONE', *, *, #3533, .T. ) ;
#4622 = CYLINDRICAL_SURFACE ( 'NONE', #1785, 250.1999999999999602 ) ;
#4623 = ORIENTED_EDGE ( 'NONE', *, *, #3273, .T. ) ;
#4624 = CARTESIAN_POINT ( 'NONE',  ( -244.4597039919655117, 8.419215816066659031, -8.199143449616464352 ) ) ;
#4625 = ORIENTED_EDGE ( 'NONE', *, *, #4600, .T. ) ;
#4626 = EDGE_CURVE ( 'NONE', #12401, #379, #4302, .T. ) ;
#4627 = DIRECTION ( 'NONE',  ( 1.000000000000000000, 0.000000000000000000, 0.000000000000000000 ) ) ;
#4628 = CARTESIAN_POINT ( 'NONE',  ( 71.82423009839129691, 19.40000000000000213, 197.3354503650404865 ) ) ;
#4629 = CARTESIAN_POINT ( 'NONE',  ( -249.7999494874248398, -11.99892863383222874, -1.190337990051804296 ) ) ;
#4630 = VECTOR ( 'NONE', #2603, 1000.000000000000000 ) ;
#4631 = CARTESIAN_POINT ( 'NONE',  ( 294.8238222686199492, -18.00000000000000000, 32.70078231946946090 ) ) ;
#4632 = AXIS2_PLACEMENT_3D ( 'NONE', #881, #2799, #10012 ) ;
#4633 = CARTESIAN_POINT ( 'NONE',  ( 0.000000000000000000, 0.000000000000000000, 0.000000000000000000 ) ) ;
#4634 = DIRECTION ( 'NONE',  ( -0.000000000000000000, -1.000000000000000000, 0.000000000000000000 ) ) ;
#4635 = ITEM_DEFINED_TRANSFORMATION ( 'NONE', 'NONE', #12309,  #805 ) ;
#4636 = CARTESIAN_POINT ( 'NONE',  ( 27.68945685411497593, -30.00000000000000000, -290.6841825403026291 ) ) ;
#4637 = EDGE_LOOP ( 'NONE', ( #12884, #3187, #3867, #9831 ) ) ;
#4638 = AXIS2_PLACEMENT_3D ( 'NONE', #2111, #7446, #10242 ) ;
#4639 = ADVANCED_FACE ( 'NONE', ( #3253 ), #4061, .F. ) ;
#4640 = ORIENTED_EDGE ( 'NONE', *, *, #8577, .T. ) ;
#4641 = CARTESIAN_POINT ( 'NONE',  ( -249.6767732310697454, -11.18100465982222502, -3.612153022818042736 ) ) ;
#4642 = CONICAL_SURFACE ( 'NONE', #9757, 5.500000000000007994, 0.7853981633974461696 ) ;
#4643 = ORIENTED_EDGE ( 'NONE', *, *, #7170, .T. ) ;
#4644 = CIRCLE ( 'NONE', #618, 5.499999999999998224 ) ;
#4645 = CARTESIAN_POINT ( 'NONE',  ( -207.6469600131875666, 19.96883746078517774, 159.3024069659174984 ) ) ;
#4646 = DIRECTION ( 'NONE',  ( -0.5469441386039890496, 0.000000000000000000, 0.8371691043312220470 ) ) ;
#4647 = DIRECTION ( 'NONE',  ( 0.000000000000000000, -1.000000000000000000, 0.000000000000000000 ) ) ;
#4648 = CIRCLE ( 'NONE', #8071, 6.500000000000005329 ) ;
#4649 = AXIS2_PLACEMENT_3D ( 'NONE', #6203, #11266, #2129 ) ;
#4650 = CARTESIAN_POINT ( 'NONE',  ( 235.0999999999999943, 0.000000000000000000, 0.000000000000000000 ) ) ;
#4651 = DIRECTION ( 'NONE',  ( 0.7709731485165535192, 0.000000000000000000, -0.6368676505102707219 ) ) ;
#4652 = ADVANCED_FACE ( 'NONE', ( #6136 ), #12135, .T. ) ;
#4653 = AXIS2_PLACEMENT_3D ( 'NONE', #456, #2313, #2255 ) ;
#4654 = LINE ( 'NONE', #8734, #7501 ) ;
#4655 = CARTESIAN_POINT ( 'NONE',  ( -29.59329699131369651, -138.4705547276867321, -29.59329699131400915 ) ) ;
#4656 = LINE ( 'NONE', #10863, #5859 ) ;
#4657 = CONICAL_SURFACE ( 'NONE', #839, 5.500000000000005329, 0.7853981633974461696 ) ;
#4658 = CARTESIAN_POINT ( 'NONE',  ( -249.7806011016498928, 11.58204051030000947, 1.980500725882820445 ) ) ;
#4659 = DIRECTION ( 'NONE',  ( 0.6368676505102716101, 0.000000000000000000, 0.7709731485165527420 ) ) ;
#4660 = CARTESIAN_POINT ( 'NONE',  ( -229.7627910449494664, -5.948779906797049932, 10.44832732976153800 ) ) ;
#4661 = VERTEX_POINT ( 'NONE', #3119 ) ;
#4662 = EDGE_LOOP ( 'NONE', ( #10223, #3763, #6778, #5461 ) ) ;
#4663 = CIRCLE ( 'NONE', #3603, 6.500000000000005329 ) ;
#4664 = DIRECTION ( 'NONE',  ( -0.000000000000000000, -1.000000000000000000, 0.000000000000000000 ) ) ;
#4665 = CARTESIAN_POINT ( 'NONE',  ( 0.000000000000000000, -1.848645179579245124, 0.000000000000000000 ) ) ;
#4666 = CIRCLE ( 'NONE', #5747, 240.3921568627449687 ) ;
#4667 = EDGE_CURVE ( 'NONE', #3975, #900, #1967, .T. ) ;
#4668 = CARTESIAN_POINT ( 'NONE',  ( -259.0935598604229995, 20.79694577620878704, -34.13493237027169158 ) ) ;
#4669 = EDGE_CURVE ( 'NONE', #4809, #953, #9425, .T. ) ;
#4670 = DIRECTION ( 'NONE',  ( 0.000000000000000000, -1.000000000000000000, 0.000000000000000000 ) ) ;
#4671 = DIRECTION ( 'NONE',  ( -0.08715574274765156004, 0.000000000000000000, -0.9961946980917461003 ) ) ;
#4672 = LINE ( 'NONE', #7808, #1777 ) ;
#4673 = AXIS2_PLACEMENT_3D ( 'NONE', #8606, #10660, #1534 ) ;
#4674 = EDGE_LOOP ( 'NONE', ( #10313, #5793 ) ) ;
#4675 = EDGE_CURVE ( 'NONE', #7886, #534, #3661, .T. ) ;
#4676 = AXIS2_PLACEMENT_3D ( 'NONE', #11260, #1129, #1934 ) ;
#4677 = DIRECTION ( 'NONE',  ( 0.000000000000000000, 0.000000000000000000, 1.000000000000000000 ) ) ;
#4678 = ORIENTED_EDGE ( 'NONE', *, *, #6647, .F. ) ;
#4679 = EDGE_LOOP ( 'NONE', ( #9829, #8393, #8109, #1563 ) ) ;
#4680 = CARTESIAN_POINT ( 'NONE',  ( 225.7689075324037162, 20.08915143297736705, -130.3442252640562913 ) ) ;
#4681 = EDGE_LOOP ( 'NONE', ( #2488, #9270 ) ) ;
#4682 = AXIS2_PLACEMENT_3D ( 'NONE', #5473, #3269, #11552 ) ;
#4683 = FACE_OUTER_BOUND ( 'NONE', #4885, .T. ) ;
#4684 = CARTESIAN_POINT ( 'NONE',  ( -197.8197553893924976, 18.00000000000000000, -64.27553482998719403 ) ) ;
#4685 = B_SPLINE_CURVE_WITH_KNOTS ( 'NONE', 3,
 ( #2994, #7076, #1697, #5765, #12694, #4753, #3556, #8829, #12893, #12072, #1942, #11273, #10332, #2135, #12275, #5062, #6210, #8346, #5336, #4198, #7275, #2206, #9407, #10266, #10198, #147, #6342, #3191 ),
 .UNSPECIFIED., .F., .F.,
 ( 4, 2, 1, 2, 2, 2, 1, 1, 2, 2, 2, 1, 1, 1, 2, 2, 4 ),
 ( 0.5011901855463575250, 0.5635414123530773089, 0.5947170257564382556, 0.6103048324581187289, 0.6258926391597992023, 0.6882438659665208736, 0.7194194793698815982, 0.7350072860715587408, 0.7428011894223938150, 0.7505950927732287781, 0.8129463195799428998, 0.8441219329832998497, 0.8597097396849784356, 0.8675036430358130657, 0.8714005947112304362, 0.8752975463866476957, 1.000000000000000000 ),
 .UNSPECIFIED. ) ;
#4686 = CARTESIAN_POINT ( 'NONE',  ( 0.000000000000000000, 3.327561323230765034, 0.000000000000000000 ) ) ;
#4687 = LINE ( 'NONE', #10069, #2449 ) ;
#4688 = ADVANCED_FACE ( 'NONE', ( #9332 ), #2108, .F. ) ;
#4689 = CARTESIAN_POINT ( 'NONE',  ( 150.6801963096165764, -28.60000000000000142, 241.8445669022807181 ) ) ;
#4690 = DIRECTION ( 'NONE',  ( 0.000000000000000000, 1.000000000000000000, 0.000000000000000000 ) ) ;
#4691 = CONTEXT_DEPENDENT_SHAPE_REPRESENTATION ( #12315, #1021 ) ;
#4692 = ORIENTED_EDGE ( 'NONE', *, *, #5816, .T. ) ;
#4693 = DIRECTION ( 'NONE',  ( 0.000000000000000000, 0.000000000000000000, -1.000000000000000000 ) ) ;
#4694 = ORIENTED_EDGE ( 'NONE', *, *, #3356, .T. ) ;
#4695 = CARTESIAN_POINT ( 'NONE',  ( -241.3472527820971152, 5.384021912553072831, -10.44389002222748886 ) ) ;
#4696 = ORIENTED_EDGE ( 'NONE', *, *, #6394, .F. ) ;
#4697 = EDGE_LOOP ( 'NONE', ( #7287, #3202 ) ) ;
#4698 = DIRECTION ( 'NONE',  ( 0.000000000000000000, 1.000000000000000000, 0.000000000000000000 ) ) ;
#4699 = CARTESIAN_POINT ( 'NONE',  ( 233.5975020798683204, 2.199572672675505824, -0.04335963121535980208 ) ) ;
#4700 = DIRECTION ( 'NONE',  ( 0.000000000000000000, 0.000000000000000000, 1.000000000000000000 ) ) ;
#4701 = FACE_BOUND ( 'NONE', #9566, .T. ) ;
#4702 = AXIS2_PLACEMENT_3D ( 'NONE', #1236, #1433, #3350 ) ;
#4703 = CARTESIAN_POINT ( 'NONE',  ( -245.5556485997495031, -9.020247694314779352, 7.914083889440647113 ) ) ;
#4704 = ORIENTED_EDGE ( 'NONE', *, *, #9961, .F. ) ;
#4705 = CYLINDRICAL_SURFACE ( 'NONE', #5650, 5.500000000000015099 ) ;
#4706 = ITEM_DEFINED_TRANSFORMATION ( 'NONE', 'NONE', #8900,  #805 ) ;
#4707 = EDGE_LOOP ( 'NONE', ( #1415, #4010, #3087, #676 ) ) ;
#4708 = CARTESIAN_POINT ( 'NONE',  ( -229.6889200636375108, 1.000000000000000000, 11.95826074310140008 ) ) ;
#4709 = ORIENTED_EDGE ( 'NONE', *, *, #6048, .F. ) ;
#4710 = CARTESIAN_POINT ( 'NONE',  ( -249.2664547940505884, -10.49941023134739915, -5.274932156554418938 ) ) ;
#4711 = EDGE_LOOP ( 'NONE', ( #6056, #793, #12913, #4781 ) ) ;
#4712 = CARTESIAN_POINT ( 'NONE',  ( -130.9697226067400493, 20.55460285172577883, 226.7975291057999527 ) ) ;
#4713 = CARTESIAN_POINT ( 'NONE',  ( 235.0999999999999943, -0.05419953901919974393, -2.749465840844381948 ) ) ;
#4714 = CARTESIAN_POINT ( 'NONE',  ( -228.6269314446401211, -30.00000000000000000, 181.7250016321579835 ) ) ;
#4715 = PRODUCT_DEFINITION_SHAPE ( 'NONE', 'NONE',  #13190 ) ;
#4716 = CARTESIAN_POINT ( 'NONE',  ( 0.000000000000000000, 22.00000000000000000, -249.2999999999999829 ) ) ;
#4717 = AXIS2_PLACEMENT_3D ( 'NONE', #240, #3557, #4298 ) ;
#4718 = ADVANCED_FACE ( 'NONE', ( #8274 ), #659, .F. ) ;
#4719 = CARTESIAN_POINT ( 'NONE',  ( -239.7946578092521577, -2.116498006235906892, 11.55893420607609912 ) ) ;
#4720 = ADVANCED_FACE ( 'NONE', ( #2988 ), #11483, .F. ) ;
#4721 = FACE_OUTER_BOUND ( 'NONE', #2554, .T. ) ;
#4722 = CARTESIAN_POINT ( 'NONE',  ( 32.05991134143148713, -138.4705547276867321, -26.90145978217099199 ) ) ;
#4723 = CARTESIAN_POINT ( 'NONE',  ( -229.9691690360902498, -11.13075325490934020, -3.783731615047171370 ) ) ;
#4724 = AXIS2_PLACEMENT_3D ( 'NONE', #13003, #872, #677 ) ;
#4725 = ITEM_DEFINED_TRANSFORMATION ( 'NONE', 'NONE', #8327,  #805 ) ;
#4726 = PRODUCT_DEFINITION_SHAPE ( 'NONE', 'NONE',  #13149 ) ;
#4727 = CARTESIAN_POINT ( 'NONE',  ( -248.3532242375468684, 9.880481159981247430, -6.359788945912696612 ) ) ;
#4728 = CARTESIAN_POINT ( 'NONE',  ( -241.2922373264150906, -5.318940986358126288, -10.75680814014601872 ) ) ;
#4729 = CARTESIAN_POINT ( 'NONE',  ( -229.9954967225296514, -11.91353440303754319, -1.485748047147350537 ) ) ;
#4730 = AXIS2_PLACEMENT_3D ( 'NONE', #7277, #4571, #8349 ) ;
#4731 = EDGE_LOOP ( 'NONE', ( #8673, #6174 ) ) ;
#4732 = ORIENTED_EDGE ( 'NONE', *, *, #6091, .F. ) ;
#4733 = FACE_OUTER_BOUND ( 'NONE', #821, .T. ) ;
#4734 = LINE ( 'NONE', #8810, #2825 ) ;
#4735 = AXIS2_PLACEMENT_3D ( 'NONE', #3198, #6346, #5271 ) ;
#4736 = CARTESIAN_POINT ( 'NONE',  ( 159.4136521835074802, 20.55460285095908191, 207.7919029867859422 ) ) ;
#4737 = DIRECTION ( 'NONE',  ( 0.000000000000000000, 1.000000000000000000, 0.000000000000000000 ) ) ;
#4738 = CARTESIAN_POINT ( 'NONE',  ( 0.000000000000000000, 0.000000000000000000, 0.000000000000000000 ) ) ;
#4739 = FACE_OUTER_BOUND ( 'NONE', #8566, .T. ) ;
#4740 = DIRECTION ( 'NONE',  ( 1.000000000000000000, 0.000000000000000000, 0.000000000000000000 ) ) ;
#4741 = ORIENTED_EDGE ( 'NONE', *, *, #119, .F. ) ;
#4742 = CARTESIAN_POINT ( 'NONE',  ( 226.1499999999999773, 1.749660080537334128, -0.03449061573949074866 ) ) ;
#4743 = ORIENTED_EDGE ( 'NONE', *, *, #7766, .T. ) ;
#4744 = VERTEX_POINT ( 'NONE', #533 ) ;
#4745 = ADVANCED_FACE ( 'NONE', ( #8468 ), #1687, .F. ) ;
#4746 = AXIS2_PLACEMENT_3D ( 'NONE', #4364, #11506, #2235 ) ;
#4747 = CONICAL_SURFACE ( 'NONE', #10922, 5.500000000000007994, 0.7853981633974461696 ) ;
#4748 = ADVANCED_FACE ( 'NONE', ( #7653 ), #7008, .F. ) ;
#4749 = CARTESIAN_POINT ( 'NONE',  ( 59.19439222780480492, 20.08915143297736705, 253.8843055347117001 ) ) ;
#4750 = EDGE_LOOP ( 'NONE', ( #8295, #11011, #903, #2738, #8035 ) ) ;
#4751 = CONICAL_SURFACE ( 'NONE', #6042, 5.499999999999998224, 0.7853981633974461696 ) ;
#4752 = DIRECTION ( 'NONE',  ( 0.000000000000000000, 0.01970892327970883220, 0.9998057603070481525 ) ) ;
#4753 = CARTESIAN_POINT ( 'NONE',  ( 239.0147185140185115, -0.4456008732492039437, -3.471580854532841709 ) ) ;
#4754 = CARTESIAN_POINT ( 'NONE',  ( -196.2980642832790181, 20.08915143307791951, 172.1812796672794832 ) ) ;
#4755 = DIRECTION ( 'NONE',  ( -0.000000000000000000, -1.000000000000000000, 0.000000000000000000 ) ) ;
#4756 = CARTESIAN_POINT ( 'NONE',  ( -220.9845196385168435, -30.00000000000000000, 190.9766794143566528 ) ) ;
#4757 = PRODUCT_DEFINITION_SHAPE ( 'NONE', 'NONE',  #13071 ) ;
#4758 = VECTOR ( 'NONE', #5269, 1000.000000000000227 ) ;
#4759 = ORIENTED_EDGE ( 'NONE', *, *, #7196, .F. ) ;
#4760 = AXIS2_PLACEMENT_3D ( 'NONE', #12597, #7533, #11926 ) ;
#4761 = FACE_OUTER_BOUND ( 'NONE', #5926, .T. ) ;
#4762 = ORIENTED_EDGE ( 'NONE', *, *, #464, .F. ) ;
#4763 = CARTESIAN_POINT ( 'NONE',  ( -243.6657758070387843, 7.864920305444456972, -8.729522397915381760 ) ) ;
#4764 = ORIENTED_EDGE ( 'NONE', *, *, #4508, .F. ) ;
#4765 = EDGE_CURVE ( 'NONE', #7894, #5570, #5590, .T. ) ;
#4766 = CIRCLE ( 'NONE', #7331, 6.500000000000005329 ) ;
#4767 = DIRECTION ( 'NONE',  ( 0.000000000000000000, 1.000000000000000000, 0.000000000000000000 ) ) ;
#4768 = CARTESIAN_POINT ( 'NONE',  ( 153.9282213272189495, -19.40000000000000213, 245.7765299597151341 ) ) ;
#4769 = DIRECTION ( 'NONE',  ( -0.6368676505102707219, 0.000000000000000000, -0.7709731485165535192 ) ) ;
#4770 = CIRCLE ( 'NONE', #11161, 6.500000000000026645 ) ;
#4771 = CARTESIAN_POINT ( 'NONE',  ( -229.7836540530505829, 6.220351915703449919, -9.975897099602894613 ) ) ;
#4772 = EDGE_CURVE ( 'NONE', #2640, #10885, #4444, .T. ) ;
#4773 = PLANE ( 'NONE',  #3064 ) ;
#4774 = CARTESIAN_POINT ( 'NONE',  ( -244.8469727609692370, -8.653369516671046924, 8.313800303729999897 ) ) ;
#4775 = CARTESIAN_POINT ( 'NONE',  ( -238.9270525397529070, 1.044268037043195374, -11.95485691270613593 ) ) ;
#4776 = ITEM_DEFINED_TRANSFORMATION ( 'NONE', 'NONE', #4849,  #805 ) ;
#4777 = EDGE_LOOP ( 'NONE', ( #9900, #2953, #10450, #6156 ) ) ;
#4778 = CARTESIAN_POINT ( 'NONE',  ( -229.9988754446348196, 11.97852054161528024, -0.7430525309543891677 ) ) ;
#4779 = VECTOR ( 'NONE', #1983, 1000.000000000000227 ) ;
#4780 = ORIENTED_EDGE ( 'NONE', *, *, #6630, .T. ) ;
#4781 = ORIENTED_EDGE ( 'NONE', *, *, #5385, .T. ) ;
#4782 = CARTESIAN_POINT ( 'NONE',  ( -249.6197023358011222, -11.04161720068388952, -4.018949317641925312 ) ) ;
#4783 = ORIENTED_EDGE ( 'NONE', *, *, #12471, .T. ) ;
#4784 = CARTESIAN_POINT ( 'NONE',  ( 207.7919029844146053, 20.55460285114793351, 159.4136521835094413 ) ) ;
#4785 = CARTESIAN_POINT ( 'NONE',  ( 197.8197553893915028, 30.00000000000000000, -58.77553482998990830 ) ) ;
#4786 = CARTESIAN_POINT ( 'NONE',  ( 11.00000000000000000, 0.000000000000000000, 250.0000000000000000 ) ) ;
#4787 = LINE ( 'NONE', #667, #9724 ) ;
#4788 = CIRCLE ( 'NONE', #12252, 2.000000000000000444 ) ;
#4789 = VECTOR ( 'NONE', #6717, 1000.000000000000000 ) ;
#4790 = CARTESIAN_POINT ( 'NONE',  ( -241.8394219714712108, 6.081466911235927419, 10.34544425800572398 ) ) ;
#4791 = DIRECTION ( 'NONE',  ( -0.5351817705578507667, 0.5538822189107470706, -0.6378047977532554924 ) ) ;
#4792 = CARTESIAN_POINT ( 'NONE',  ( 229.9973173948202430, 3.320200122780408325, -1.130823014037518170 ) ) ;
#4793 = CONTEXT_DEPENDENT_SHAPE_REPRESENTATION ( #8120, #699 ) ;
#4794 = CARTESIAN_POINT ( 'NONE',  ( -249.7944461413453894, 11.69162236983806835, -1.179780665110756521 ) ) ;
#4795 = CARTESIAN_POINT ( 'NONE',  ( -240.4404613007271507, -3.704209566672288290, -11.41407139955809669 ) ) ;
#4796 = AXIS2_PLACEMENT_3D ( 'NONE', #3679, #2670, #11951 ) ;
#4797 =( REPRESENTATION_RELATIONSHIP ('NONE','NONE', #12019, #182 ) REPRESENTATION_RELATIONSHIP_WITH_TRANSFORMATION ( #1243 )SHAPE_REPRESENTATION_RELATIONSHIP( ) );
#4798 = CARTESIAN_POINT ( 'NONE',  ( -229.9999900080290729, -11.99981304996879850, -0.3780019861745291809 ) ) ;
#4799 = ORIENTED_EDGE ( 'NONE', *, *, #7048, .T. ) ;
#4800 = VERTEX_POINT ( 'NONE', #10726 ) ;
#4801 = EDGE_CURVE ( 'NONE', #167, #3488, #1475, .T. ) ;
#4802 = DIRECTION ( 'NONE',  ( -0.000000000000000000, -1.000000000000000000, 0.000000000000000000 ) ) ;
#4803 = FACE_OUTER_BOUND ( 'NONE', #10689, .T. ) ;
#4804 = CARTESIAN_POINT ( 'NONE',  ( 67.76049180374880621, 20.55460285150727273, 252.9796497720274147 ) ) ;
#4805 = CARTESIAN_POINT ( 'NONE',  ( 220.3999999999999773, 0.000000000000000000, 0.000000000000000000 ) ) ;
#4806 = CARTESIAN_POINT ( 'NONE',  ( 0.000000000000000000, 0.000000000000000000, 0.000000000000000000 ) ) ;
#4807 = CARTESIAN_POINT ( 'NONE',  ( -185.9653539489998195, -19.00000000000000000, -225.1241593668329699 ) ) ;
#4808 = CARTESIAN_POINT ( 'NONE',  ( 0.000000000000000000, 29.00000000000000000, -202.4999999999999716 ) ) ;
#4809 = VERTEX_POINT ( 'NONE', #10655 ) ;
#4810 = CARTESIAN_POINT ( 'NONE',  ( -239.6697886840235583, -1.970929121827114106, 11.83704280384634266 ) ) ;
#4811 = VERTEX_POINT ( 'NONE', #4450 ) ;
#4812 = ORIENTED_EDGE ( 'NONE', *, *, #9998, .T. ) ;
#4813 = ADVANCED_FACE ( 'NONE', ( #10529 ), #10193, .F. ) ;
#4814 = DIRECTION ( 'NONE',  ( 0.4503334343941555740, 0.7071067811865490160, 0.5451603414287971017 ) ) ;
#4815 = ORIENTED_EDGE ( 'NONE', *, *, #1603, .F. ) ;
#4816 = FACE_OUTER_BOUND ( 'NONE', #2290, .T. ) ;
#4817 = CARTESIAN_POINT ( 'NONE',  ( -234.1947771733725006, 20.08915143296620442, 115.4648407707744013 ) ) ;
#4818 = CARTESIAN_POINT ( 'NONE',  ( 7.960204194457795477E-16, 30.00000000000000000, 201.4999999999999716 ) ) ;
#4819 = FILL_AREA_STYLE ('',( #7696 ) ) ;
#4820 = ADVANCED_FACE ( 'NONE', ( #12463 ), #5081, .F. ) ;
#4821 = EDGE_CURVE ( 'NONE', #7406, #11365, #1047, .T. ) ;
#4822 = ORIENTED_EDGE ( 'NONE', *, *, #8129, .T. ) ;
#4823 = CARTESIAN_POINT ( 'NONE',  ( 0.000000000000000000, 21.94174202707280941, 0.000000000000000000 ) ) ;
#4824 = ORIENTED_EDGE ( 'NONE', *, *, #8325, .F. ) ;
#4825 = DIRECTION ( 'NONE',  ( 0.000000000000000000, 0.000000000000000000, -1.000000000000000000 ) ) ;
#4826 = VERTEX_POINT ( 'NONE', #6600 ) ;
#4827 = AXIS2_PLACEMENT_3D ( 'NONE', #933, #9061, #10927 ) ;
#4828 = CARTESIAN_POINT ( 'NONE',  ( 240.1881190901118259, -2.326983775948836985, -2.614448608526312334 ) ) ;
#4829 = SURFACE_STYLE_USAGE ( .BOTH. , #48 ) ;
#4830 = DIRECTION ( 'NONE',  ( 0.000000000000000000, 0.000000000000000000, 1.000000000000000000 ) ) ;
#4831 = CARTESIAN_POINT ( 'NONE',  ( 229.9000000000000057, -0.07883569311883599495, -3.999223041228192610 ) ) ;
#4832 = CARTESIAN_POINT ( 'NONE',  ( -130.3442252640568029, 20.08915143297736705, 225.7689075324034036 ) ) ;
#4833 = PRODUCT_DEFINITION_SHAPE ( 'NONE', 'NONE',  #13118 ) ;
#4834 = CARTESIAN_POINT ( 'NONE',  ( -242.3253012572137948, -6.649486011330081325, 9.989214338957303596 ) ) ;
#4835 = ADVANCED_FACE ( 'NONE', ( #266 ), #9764, .F. ) ;
#4836 = CONICAL_SURFACE ( 'NONE', #6972, 249.0000000000000284, 1.373400766945015894 ) ;
#4837 = EDGE_CURVE ( 'NONE', #12496, #1017, #7859, .T. ) ;
#4838 = CARTESIAN_POINT ( 'NONE',  ( -239.0407087265602399, 1.256038988924583988, -11.93408471340098664 ) ) ;
#4839 = CONTEXT_DEPENDENT_SHAPE_REPRESENTATION ( #12127, #12353 ) ;
#4840 = ORIENTED_EDGE ( 'NONE', *, *, #11342, .F. ) ;
#4841 = CARTESIAN_POINT ( 'NONE',  ( -239.1938262371573103, -1.469859134671393397, -11.65770207259568281 ) ) ;
#4842 = ITEM_DEFINED_TRANSFORMATION ( 'NONE', 'NONE', #5337,  #805 ) ;
#4843 = EDGE_LOOP ( 'NONE', ( #1526, #562, #4812, #4822 ) ) ;
#4844 = B_SPLINE_CURVE_WITH_KNOTS ( 'NONE', 3,
 ( #4101, #7978, #12042, #9907, #2757, #2893, #5096, #3026, #1910, #11169, #7904, #12103, #2827 ),
 .UNSPECIFIED., .F., .F.,
 ( 4, 2, 2, 1, 2, 2, 4 ),
 ( 0.000000000000000000, 0.2500000000000368594, 0.3750000000000559552, 0.4375000000000651701, 0.4687500000000694445, 0.5000000000000737188, 1.000000000000000000 ),
 .UNSPECIFIED. ) ;
#4845 = EDGE_CURVE ( 'NONE', #953, #8825, #10463, .T. ) ;
#4846 = ORIENTED_EDGE ( 'NONE', *, *, #10380, .F. ) ;
#4847 = CARTESIAN_POINT ( 'NONE',  ( -249.7718704162269319, -11.53079704007455142, -2.260598008543511561 ) ) ;
#4848 = EDGE_LOOP ( 'NONE', ( #6896, #4451 ) ) ;
#4849 = AXIS2_PLACEMENT_3D ( 'NONE', #8302, #11293, #2157 ) ;
#4850 = CARTESIAN_POINT ( 'NONE',  ( 259.6535381495593242, 20.55460285082940075, -34.20858920423904692 ) ) ;
#4851 = DIRECTION ( 'NONE',  ( 0.000000000000000000, 1.000000000000000000, 0.000000000000000000 ) ) ;
#4852 = CARTESIAN_POINT ( 'NONE',  ( 197.8197553893920144, 30.00000000000000000, 58.77553482998850853 ) ) ;
#4853 = DIRECTION ( 'NONE',  ( 0.000000000000000000, 0.9998057603070480415, -0.01970892327970899874 ) ) ;
#4854 = B_SPLINE_CURVE_WITH_KNOTS ( 'NONE', 3,
 ( #5182, #4053, #10119, #10317 ),
 .UNSPECIFIED., .F., .F.,
 ( 4, 4 ),
 ( 0.000000000000000000, 1.000000000000000000 ),
 .UNSPECIFIED. ) ;
#4855 = CARTESIAN_POINT ( 'NONE',  ( -239.6752751780977064, -1.974315850609194012, 11.58364238450984018 ) ) ;
#4856 = CARTESIAN_POINT ( 'NONE',  ( 157.1762463448213225, -28.60000000000000142, 249.7084930171495785 ) ) ;
#4857 = DIRECTION ( 'NONE',  ( 0.3518698652246443626, 0.5538822189107470706, -0.7545873610930001751 ) ) ;
#4858 = VECTOR ( 'NONE', #5965, 1000.000000000000000 ) ;
#4859 = CIRCLE ( 'NONE', #4638, 5.100000000000000533 ) ;
#4860 = CARTESIAN_POINT ( 'NONE',  ( -0.000000000000000000, -30.00000000000000000, 0.000000000000000000 ) ) ;
#4861 = CIRCLE ( 'NONE', #3792, 250.1999999999999602 ) ;
#4862 = AXIS2_PLACEMENT_3D ( 'NONE', #6948, #5402, #12529 ) ;
#4863 = ITEM_DEFINED_TRANSFORMATION ( 'NONE', 'NONE', #5756,  #805 ) ;
#4864 = AXIS2_PLACEMENT_3D ( 'NONE', #4336, #7475, #10664 ) ;
#4865 = AXIS2_PLACEMENT_3D ( 'NONE', #3682, #2552, #500 ) ;
#4866 = CARTESIAN_POINT ( 'NONE',  ( -249.7900429581053743, 11.65124970777654667, -1.521630442913122216 ) ) ;
#4867 = CARTESIAN_POINT ( 'NONE',  ( -229.7804030572558247, -6.567824493990499057, -10.05005982919573881 ) ) ;
#4868 = EDGE_LOOP ( 'NONE', ( #1231, #12804, #12420, #1672 ) ) ;
#4869 = ORIENTED_EDGE ( 'NONE', *, *, #12723, .T. ) ;
#4870 = LINE ( 'NONE', #809, #4153 ) ;
#4871 = FACE_BOUND ( 'NONE', #3759, .T. ) ;
#4872 = PRODUCT_DEFINITION_SHAPE ( 'NONE', 'NONE',  #13082 ) ;
#4873 = CARTESIAN_POINT ( 'NONE',  ( 34.13493236988740165, 20.79694577678859702, 259.0935598591244684 ) ) ;
#4874 = FACE_OUTER_BOUND ( 'NONE', #11957, .T. ) ;
#4875 = CIRCLE ( 'NONE', #1473, 6.500000000000005329 ) ;
#4876 = CARTESIAN_POINT ( 'NONE',  ( 0.000000000000000000, 0.000000000000000000, 0.000000000000000000 ) ) ;
#4877 = DIRECTION ( 'NONE',  ( 0.6368676505102707219, 0.000000000000000000, 0.7709731485165536302 ) ) ;
#4878 = CIRCLE ( 'NONE', #10629, 254.1999999999999886 ) ;
#4879 = EDGE_CURVE ( 'NONE', #10920, #11715, #6533, .T. ) ;
#4880 = VERTEX_POINT ( 'NONE', #11537 ) ;
#4881 = DIRECTION ( 'NONE',  ( 0.000000000000000000, 0.9998057603070481525, -0.01970892327970899874 ) ) ;
#4882 = UNCERTAINTY_MEASURE_WITH_UNIT (LENGTH_MEASURE( 1.000000000000000082E-05 ), #2562, 'distance_accuracy_value', 'NONE');
#4883 = AXIS2_PLACEMENT_3D ( 'NONE', #9908, #781, #4830 ) ;
#4884 = CARTESIAN_POINT ( 'NONE',  ( -239.4330563949805537, -1.762617345644425404, 11.86984317963793778 ) ) ;
#4885 = EDGE_LOOP ( 'NONE', ( #9916, #11045, #7637, #13004 ) ) ;
#4886 = VERTEX_POINT ( 'NONE', #5330 ) ;
#4887 = PRODUCT_DEFINITION_CONTEXT ( 'detailed design', #9326, 'design' ) ;
#4888 = FACE_OUTER_BOUND ( 'NONE', #2410, .T. ) ;
#4889 = VERTEX_POINT ( 'NONE', #6667 ) ;
#4890 = CYLINDRICAL_SURFACE ( 'NONE', #10713, 249.7999999999999829 ) ;
#4891 = CARTESIAN_POINT ( 'NONE',  ( -1.009475258464312158E-12, 20.08915143297736350, 260.5542428351129729 ) ) ;
#4892 = CARTESIAN_POINT ( 'NONE',  ( -239.8750565963660506, -2.115697797198144769, -11.81209311402866646 ) ) ;
#4893 = CARTESIAN_POINT ( 'NONE',  ( 287.1814104624967854, -19.00000000000000000, 23.44910453727081290 ) ) ;
#4894 = EDGE_CURVE ( 'NONE', #8752, #9436, #12593, .T. ) ;
#4895 = EDGE_CURVE ( 'NONE', #1370, #10870, #2320, .T. ) ;
#4896 = EDGE_LOOP ( 'NONE', ( #2050, #9520, #7869, #5491 ) ) ;
#4897 = DIRECTION ( 'NONE',  ( 0.000000000000000000, 0.9998057603070481525, -0.01970892327970899874 ) ) ;
#4898 = ORIENTED_EDGE ( 'NONE', *, *, #7024, .F. ) ;
#4899 = CARTESIAN_POINT ( 'NONE',  ( -246.6527294682080367, 9.457576189755920737, -6.972573804798820163 ) ) ;
#4900 = ORIENTED_EDGE ( 'NONE', *, *, #12793, .F. ) ;
#4901 = EDGE_CURVE ( 'NONE', #4811, #13033, #12540, .T. ) ;
#4902 = DIRECTION ( 'NONE',  ( 1.000000000000000000, -0.000000000000000000, 1.224646799147353207E-16 ) ) ;
#4903 = CARTESIAN_POINT ( 'NONE',  ( -122.2593324768321992, 18.00000000000000000, 168.2755348299905052 ) ) ;
#4904 = FACE_OUTER_BOUND ( 'NONE', #10983, .T. ) ;
#4905 = DIRECTION ( 'NONE',  ( 1.000000000000000000, 0.000000000000000000, 0.000000000000000000 ) ) ;
#4906 = CARTESIAN_POINT ( 'NONE',  ( -229.9847620420411261, 11.44809447175227035, 2.673990570740190975 ) ) ;
#4907 = CARTESIAN_POINT ( 'NONE',  ( -195.0000000000000000, 30.00000000000000000, 0.000000000000000000 ) ) ;
#4908 = CARTESIAN_POINT ( 'NONE',  ( -242.5248711350201631, -6.860954764109954418, 9.845341014195845730 ) ) ;
#4909 =( REPRESENTATION_RELATIONSHIP ('NONE','NONE', #12019, #5191 ) REPRESENTATION_RELATIONSHIP_WITH_TRANSFORMATION ( #5413 )SHAPE_REPRESENTATION_RELATIONSHIP( ) );
#4910 = CARTESIAN_POINT ( 'NONE',  ( -34.05310945291963520, 20.79694577634646180, -258.6823826759385270 ) ) ;
#4911 = ORIENTED_EDGE ( 'NONE', *, *, #3985, .T. ) ;
#4912 = DIRECTION ( 'NONE',  ( 0.000000000000000000, 0.000000000000000000, 1.000000000000000000 ) ) ;
#4913 = PRODUCT_DEFINITION_SHAPE ( 'NONE', 'NONE',  #13097 ) ;
#4914 = ORIENTED_EDGE ( 'NONE', *, *, #10186, .T. ) ;
#4915 = ORIENTED_EDGE ( 'NONE', *, *, #12321, .T. ) ;
#4916 = CARTESIAN_POINT ( 'NONE',  ( -249.7841416270006789, -11.60584252727432109, -1.834925605625155498 ) ) ;
#4917 = ORIENTED_EDGE ( 'NONE', *, *, #1252, .F. ) ;
#4918 = EDGE_CURVE ( 'NONE', #9610, #10870, #9583, .T. ) ;
#4919 = CARTESIAN_POINT ( 'NONE',  ( 17.10461161403171815, 20.55460285106647689, -261.3381329044966606 ) ) ;
#4920 = EDGE_CURVE ( 'NONE', #789, #5629, #12658, .T. ) ;
#4921 = CARTESIAN_POINT ( 'NONE',  ( -197.8197553893924976, 30.00000000000000000, -70.77553482998720824 ) ) ;
#4922 = CARTESIAN_POINT ( 'NONE',  ( 235.4000000000000057, 0.000000000000000000, 0.000000000000000000 ) ) ;
#4923 = CARTESIAN_POINT ( 'NONE',  ( -248.0831933713610056, -9.830508068705260172, -6.436117704883899115 ) ) ;
#4924 = AXIS2_PLACEMENT_3D ( 'NONE', #10976, #6845, #2038 ) ;
#4925 = CARTESIAN_POINT ( 'NONE',  ( -210.0000000000000000, 30.00000000000000000, -6.500000000000000000 ) ) ;
#4926 = CARTESIAN_POINT ( 'NONE',  ( -247.8580199589107451, 9.788721918689880397, 6.941247868350859385 ) ) ;
#4927 = DIRECTION ( 'NONE',  ( 0.000000000000000000, -1.000000000000000000, 0.000000000000000000 ) ) ;
#4928 = CARTESIAN_POINT ( 'NONE',  ( 29.59329699131410862, -138.4705547276867321, -29.59329699131359703 ) ) ;
#4929 = CARTESIAN_POINT ( 'NONE',  ( -229.7506357186298089, -4.852194303783566198, 10.70827597515549989 ) ) ;
#4930 = ITEM_DEFINED_TRANSFORMATION ( 'NONE', 'NONE', #7881,  #805 ) ;
#4931 = CARTESIAN_POINT ( 'NONE',  ( -229.6921463704719883, -1.741046932630716526, -11.89629128545617043 ) ) ;
#4932 = ORIENTED_EDGE ( 'NONE', *, *, #375, .T. ) ;
#4933 = ORIENTED_EDGE ( 'NONE', *, *, #12510, .F. ) ;
#4934 = CONICAL_SURFACE ( 'NONE', #2166, 6.500000000000005329, 0.7853981633974476129 ) ;
#4935 = CARTESIAN_POINT ( 'NONE',  ( -34.10614053585819505, 20.08915143303038775, 258.8746690719034973 ) ) ;
#4936 = ADVANCED_FACE ( 'NONE', ( #5862 ), #8932, .F. ) ;
#4937 = DIRECTION ( 'NONE',  ( 0.000000000000000000, 0.000000000000000000, -1.000000000000000000 ) ) ;
#4938 = CIRCLE ( 'NONE', #2594, 6.500000000000005329 ) ;
#4939 = DIRECTION ( 'NONE',  ( 0.000000000000000000, 0.000000000000000000, 1.000000000000000000 ) ) ;
#4940 = CARTESIAN_POINT ( 'NONE',  ( 122.2593324768346008, 30.00000000000000000, 174.7755348299889988 ) ) ;
#4941 = DIRECTION ( 'NONE',  ( 0.1736481776669374921, 0.000000000000000000, -0.9848077530122070211 ) ) ;
#4942 = AXIS2_PLACEMENT_3D ( 'NONE', #2480, #9489, #1422 ) ;
#4943 = CARTESIAN_POINT ( 'NONE',  ( -245.6300371773186839, -9.052739546058479192, 7.492707602925837485 ) ) ;
#4944 = ORIENTED_EDGE ( 'NONE', *, *, #9904, .F. ) ;
#4945 = AXIS2_PLACEMENT_3D ( 'NONE', #10398, #9701, #8715 ) ;
#4946 = LINE ( 'NONE', #8228, #1056 ) ;
#4947 = CARTESIAN_POINT ( 'NONE',  ( -239.0463147773640742, -1.265540211687415484, 11.93307915096743166 ) ) ;
#4948 = VERTEX_POINT ( 'NONE', #7919 ) ;
#4949 = EDGE_LOOP ( 'NONE', ( #12527, #2687, #12338, #5350, #12115, #12543 ) ) ;
#4950 = LINE ( 'NONE', #9028, #7003 ) ;
#4951 = DIRECTION ( 'NONE',  ( 0.6368676505102700558, 0.000000000000000000, 0.7709731485165541853 ) ) ;
#4952 = PRODUCT_DEFINITION_SHAPE ( 'NONE', 'NONE',  #13125 ) ;
#4953 = CARTESIAN_POINT ( 'NONE',  ( -249.1360723386881943, 10.36505329179906632, 5.534757212115697378 ) ) ;
#4954 = AXIS2_PLACEMENT_3D ( 'NONE', #5374, #11578, #2299 ) ;
#4955 = CARTESIAN_POINT ( 'NONE',  ( 115.7315435902013263, 19.96883745981483926, -234.7354397754176318 ) ) ;
#4956 = DIRECTION ( 'NONE',  ( -0.000000000000000000, -1.000000000000000000, 0.000000000000000000 ) ) ;
#4957 = CARTESIAN_POINT ( 'NONE',  ( -242.2371604624929944, 6.538578786594999137, 9.762666687128254139 ) ) ;
#4958 = VERTEX_POINT ( 'NONE', #2646 ) ;
#4959 = CARTESIAN_POINT ( 'NONE',  ( -239.1752428789251326, -1.444203915845354125, 11.66090825388631202 ) ) ;
#4960 = AXIS2_PLACEMENT_3D ( 'NONE', #12824, #11835, #569 ) ;
#4961 = AXIS2_PLACEMENT_3D ( 'NONE', #11314, #4373, #1186 ) ;
#4962 = EDGE_LOOP ( 'NONE', ( #3022, #12153, #5146, #1821 ) ) ;
#4963 = AXIS2_PLACEMENT_3D ( 'NONE', #3387, #8473, #9524 ) ;
#4964 = DIRECTION ( 'NONE',  ( 0.000000000000000000, -1.000000000000000000, 0.000000000000000000 ) ) ;
#4965 = ORIENTED_EDGE ( 'NONE', *, *, #3426, .F. ) ;
#4966 = EDGE_CURVE ( 'NONE', #8945, #9988, #4878, .T. ) ;
#4967 = EDGE_CURVE ( 'NONE', #4005, #11054, #11651, .T. ) ;
#4968 = CYLINDRICAL_SURFACE ( 'NONE', #2161, 5.499999999999986677 ) ;
#4969 = DIRECTION ( 'NONE',  ( 0.000000000000000000, 0.000000000000000000, 1.000000000000000000 ) ) ;
#4970 = DIRECTION ( 'NONE',  ( 0.6368676505102708330, 0.000000000000000000, 0.7709731485165535192 ) ) ;
#4971 = DIRECTION ( 'NONE',  ( 0.000000000000000000, 1.000000000000000000, 0.000000000000000000 ) ) ;
#4972 = CIRCLE ( 'NONE', #6691, 1.000000000000000000 ) ;
#4973 = CARTESIAN_POINT ( 'NONE',  ( 220.3999999999999773, 0.000000000000000000, 0.000000000000000000 ) ) ;
#4974 = CARTESIAN_POINT ( 'NONE',  ( -240.5255509705923771, -3.902938849136275756, 11.34756747380466990 ) ) ;
#4975 = CARTESIAN_POINT ( 'NONE',  ( -239.6374854881607348, 1.945441273982636776, -11.84125337015805179 ) ) ;
#4976 = ITEM_DEFINED_TRANSFORMATION ( 'NONE', 'NONE', #11028,  #805 ) ;
#4977 = ORIENTED_EDGE ( 'NONE', *, *, #4845, .F. ) ;
#4978 = DIRECTION ( 'NONE',  ( 0.000000000000000000, -1.000000000000000000, 0.000000000000000000 ) ) ;
#4979 = ORIENTED_EDGE ( 'NONE', *, *, #6793, .T. ) ;
#4980 = TOROIDAL_SURFACE ( 'NONE', #5419, 247.7999999999999829, 2.000000000000000000 ) ;
#4981 = ORIENTED_EDGE ( 'NONE', *, *, #7529, .T. ) ;
#4982 = CARTESIAN_POINT ( 'NONE',  ( -248.8555022323135120, -10.14371006989313706, 5.930260236134023977 ) ) ;
#4983 = ORIENTED_EDGE ( 'NONE', *, *, #775, .T. ) ;
#4984 = CARTESIAN_POINT ( 'NONE',  ( 34.20858920406338655, 20.55460285047751157, -259.6535381481361355 ) ) ;
#4985 = CARTESIAN_POINT ( 'NONE',  ( -247.4131856387215862, 9.690266168050630569, -7.079595847188384639 ) ) ;
#4986 = CARTESIAN_POINT ( 'NONE',  ( 3.059167704270088292E-14, 0.000000000000000000, 249.7999999999999829 ) ) ;
#4987 = DIRECTION ( 'NONE',  ( 0.000000000000000000, -1.000000000000000000, 0.000000000000000000 ) ) ;
#4988 = CARTESIAN_POINT ( 'NONE',  ( -246.0119047653037114, 9.221725595239210094, 7.678802607589900298 ) ) ;
#4989 =( REPRESENTATION_RELATIONSHIP ('NONE','NONE', #12019, #182 ) REPRESENTATION_RELATIONSHIP_WITH_TRANSFORMATION ( #2869 )SHAPE_REPRESENTATION_RELATIONSHIP( ) );
#4990 = CIRCLE ( 'NONE', #10742, 249.7999999999999829 ) ;
#4991 = PRESENTATION_STYLE_ASSIGNMENT (( #935 ) ) ;
#4992 = DIRECTION ( 'NONE',  ( -0.08715574274764852081, 0.000000000000000000, -0.9961946980917463224 ) ) ;
#4993 = ADVANCED_FACE ( 'NONE', ( #6191 ), #2948, .F. ) ;
#4994 = CARTESIAN_POINT ( 'NONE',  ( 235.4000000000000057, -1.749660080537334128, 0.03449061573949095683 ) ) ;
#4995 = CONTEXT_DEPENDENT_SHAPE_REPRESENTATION ( #6207, #4603 ) ;
#4996 = EDGE_CURVE ( 'NONE', #6924, #11433, #6594, .T. ) ;
#4997 = CARTESIAN_POINT ( 'NONE',  ( -229.9968630190249712, -11.93995442319631373, 1.297703334126907304 ) ) ;
#4998 = ORIENTED_EDGE ( 'NONE', *, *, #1303, .F. ) ;
#4999 = ORIENTED_EDGE ( 'NONE', *, *, #10537, .F. ) ;
#5000 = AXIS2_PLACEMENT_3D ( 'NONE', #2992, #9010, #876 ) ;
#5001 = CARTESIAN_POINT ( 'NONE',  ( 0.000000000000000000, 21.99999999999995381, -250.3823410207189966 ) ) ;
#5002 = DIRECTION ( 'NONE',  ( -0.000000000000000000, -1.000000000000000000, 0.000000000000000000 ) ) ;
#5003 = CARTESIAN_POINT ( 'NONE',  ( 0.000000000000000000, 19.00000000000000000, 0.000000000000000000 ) ) ;
#5004 = DIRECTION ( 'NONE',  ( 0.000000000000000000, 1.000000000000000000, 0.000000000000000000 ) ) ;
#5005 = FACE_OUTER_BOUND ( 'NONE', #11902, .T. ) ;
#5006 = DIRECTION ( 'NONE',  ( 0.3420201433256569445, 0.000000000000000000, 0.9396926207859128688 ) ) ;
#5007 = CARTESIAN_POINT ( 'NONE',  ( -241.3329571118493959, -5.362363067942219175, 10.45502706639050672 ) ) ;
#5008 = AXIS2_PLACEMENT_3D ( 'NONE', #3101, #12619, #363 ) ;
#5009 = EDGE_CURVE ( 'NONE', #10885, #2640, #3164, .T. ) ;
#5010 = ORIENTED_EDGE ( 'NONE', *, *, #6579, .F. ) ;
#5011 = CIRCLE ( 'NONE', #2453, 3.153020646647511249 ) ;
#5012 = DIRECTION ( 'NONE',  ( -0.000000000000000000, 1.000000000000000000, 0.000000000000000000 ) ) ;
#5013 = PLANE ( 'NONE',  #8288 ) ;
#5014 = ORIENTED_EDGE ( 'NONE', *, *, #5923, .F. ) ;
#5015 = ORIENTED_EDGE ( 'NONE', *, *, #1557, .T. ) ;
#5016 = EDGE_CURVE ( 'NONE', #2888, #6668, #834, .T. ) ;
#5017 = CARTESIAN_POINT ( 'NONE',  ( -31.19222893191934531, -19.00000000000000000, 286.4438302234617595 ) ) ;
#5018 = DIRECTION ( 'NONE',  ( 0.000000000000000000, -1.000000000000000000, 0.000000000000000000 ) ) ;
#5019 = CARTESIAN_POINT ( 'NONE',  ( -249.5485775754664814, 10.89766932136149613, 4.396091617827336151 ) ) ;
#5020 = CARTESIAN_POINT ( 'NONE',  ( 234.1947771726669885, 20.08915143309429041, 115.4648407708036046 ) ) ;
#5021 = CARTESIAN_POINT ( 'NONE',  ( -238.8644114632761557, -0.8921807392855528596, -11.96685057743542480 ) ) ;
#5022 =( NAMED_UNIT ( * ) SI_UNIT ( $, .STERADIAN. ) SOLID_ANGLE_UNIT ( ) );
#5023 = CARTESIAN_POINT ( 'NONE',  ( -241.4114469334947444, 5.479936497169059173, 10.39393372328349585 ) ) ;
#5024 = ORIENTED_EDGE ( 'NONE', *, *, #7704, .T. ) ;
#5025 = CARTESIAN_POINT ( 'NONE',  ( -197.8197553893924976, 19.00000000000000000, -58.77553482998720114 ) ) ;
#5026 = EDGE_LOOP ( 'NONE', ( #5195, #10986, #715, #10684 ) ) ;
#5027 = DIRECTION ( 'NONE',  ( 0.000000000000000000, 0.000000000000000000, -1.000000000000000000 ) ) ;
#5028 = VERTEX_POINT ( 'NONE', #11391 ) ;
#5029 = DIRECTION ( 'NONE',  ( 1.000000000000000000, 0.000000000000000000, 0.000000000000000000 ) ) ;
#5030 = FILL_AREA_STYLE_COLOUR ( '', #13014 ) ;
#5031 = CARTESIAN_POINT ( 'NONE',  ( 239.0028278883971780, 0.3789072388907981925, 3.479912193141485144 ) ) ;
#5032 = LINE ( 'NONE', #7113, #6012 ) ;
#5033 = CARTESIAN_POINT ( 'NONE',  ( -225.1241593668336236, -30.00000000000000000, 185.9653539489990521 ) ) ;
#5034 = DIRECTION ( 'NONE',  ( 0.000000000000000000, 1.000000000000000000, 0.000000000000000000 ) ) ;
#5035 = CARTESIAN_POINT ( 'NONE',  ( -239.6107305625394872, 1.923727078433295601, -11.84479882075283541 ) ) ;
#5036 = EDGE_LOOP ( 'NONE', ( #2046, #4743 ) ) ;
#5037 = CARTESIAN_POINT ( 'NONE',  ( -239.1925639862890591, -1.468143820144465650, -11.65791905985560284 ) ) ;
#5038 = EDGE_CURVE ( 'NONE', #12564, #2818, #1091, .T. ) ;
#5039 = ORIENTED_EDGE ( 'NONE', *, *, #2487, .F. ) ;
#5040 = CARTESIAN_POINT ( 'NONE',  ( -242.4509935382772596, -6.787150506045976250, -9.898021028433552360 ) ) ;
#5041 = CARTESIAN_POINT ( 'NONE',  ( -249.3819455667575369, -10.64000139045997351, 4.985720160815903412 ) ) ;
#5042 = ORIENTED_EDGE ( 'NONE', *, *, #3747, .F. ) ;
#5043 = CARTESIAN_POINT ( 'NONE',  ( 207.3438552934050279, 20.79694577613707551, 159.0697709850429931 ) ) ;
#5044 = CARTESIAN_POINT ( 'NONE',  ( 138.9238112054132159, -23.50000000000000000, -212.6409525001303962 ) ) ;
#5045 = CARTESIAN_POINT ( 'NONE',  ( -245.4195491721955875, -8.949151682342847636, -7.614144253697441300 ) ) ;
#5046 = CIRCLE ( 'NONE', #2281, 254.0000000000000000 ) ;
#5047 =( REPRESENTATION_RELATIONSHIP ('NONE','NONE', #12019, #182 ) REPRESENTATION_RELATIONSHIP_WITH_TRANSFORMATION ( #4635 )SHAPE_REPRESENTATION_RELATIONSHIP( ) );
#5048 = CARTESIAN_POINT ( 'NONE',  ( -246.2818250957199098, 9.328552628620979448, 7.548386157364489257 ) ) ;
#5049 =( LENGTH_UNIT ( ) NAMED_UNIT ( * ) SI_UNIT ( .MILLI., .METRE. ) );
#5050 = DIRECTION ( 'NONE',  ( 0.4162975160790887696, 0.5538822189107472926, 0.7210484489137247710 ) ) ;
#5051 = CARTESIAN_POINT ( 'NONE',  ( -229.9990560493756107, -11.73156903894478376, 0.7633253822087937568 ) ) ;
#5052 = EDGE_CURVE ( 'NONE', #6599, #1185, #4644, .T. ) ;
#5053 = ITEM_DEFINED_TRANSFORMATION ( 'NONE', 'NONE', #12143,  #805 ) ;
#5054 = PRODUCT_DEFINITION_SHAPE ( 'NONE', 'NONE',  #13110 ) ;
#5055 =( GEOMETRIC_REPRESENTATION_CONTEXT ( 3 ) GLOBAL_UNCERTAINTY_ASSIGNED_CONTEXT ( ( #6894 ) ) GLOBAL_UNIT_ASSIGNED_CONTEXT ( ( #4560, #8640, #11577 ) ) REPRESENTATION_CONTEXT ( 'NONE', 'WORKASPACE' ) );
#5056 = CARTESIAN_POINT ( 'NONE',  ( 227.3999999999999773, -0.1281080013181084831, -6.498737441995811714 ) ) ;
#5057 = ORIENTED_EDGE ( 'NONE', *, *, #10070, .T. ) ;
#5058 = ORIENTED_EDGE ( 'NONE', *, *, #3080, .T. ) ;
#5059 = CARTESIAN_POINT ( 'NONE',  ( -247.2466869557850089, 20.08915143288961858, -83.95474316020511196 ) ) ;
#5060 = DIRECTION ( 'NONE',  ( -0.6368676505102698338, 0.000000000000000000, -0.7709731485165541853 ) ) ;
#5061 = EDGE_CURVE ( 'NONE', #9111, #10034, #13021, .T. ) ;
#5062 = CARTESIAN_POINT ( 'NONE',  ( 239.1963018252558584, -1.024882057282255898, -3.346595946699232549 ) ) ;
#5063 = CONICAL_SURFACE ( 'NONE', #824, 2.250000000000000000, 0.4188790204786335125 ) ;
#5064 = CARTESIAN_POINT ( 'NONE',  ( 259.0935598587374784, 20.79694577687060786, 34.13493237085509691 ) ) ;
#5065 = AXIS2_PLACEMENT_3D ( 'NONE', #9881, #758, #6887 ) ;
#5066 = CARTESIAN_POINT ( 'NONE',  ( -233.0000000000000000, 1.000000000000000000, -12.50000000000000000 ) ) ;
#5067 = CARTESIAN_POINT ( 'NONE',  ( -241.0175249738750551, -4.851820797546724684, 10.70187039113691085 ) ) ;
#5068 = CONTEXT_DEPENDENT_SHAPE_REPRESENTATION ( #10015, #2084 ) ;
#5069 = ORIENTED_EDGE ( 'NONE', *, *, #3028, .F. ) ;
#5070 = DIRECTION ( 'NONE',  ( 1.000000000000000000, 0.000000000000000000, 0.000000000000000000 ) ) ;
#5071 = CARTESIAN_POINT ( 'NONE',  ( 229.9999987649675859, -3.499918840721679025, 0.2295273192198076240 ) ) ;
#5072 = ORIENTED_EDGE ( 'NONE', *, *, #3621, .T. ) ;
#5073 = ORIENTED_EDGE ( 'NONE', *, *, #10116, .F. ) ;
#5074 = AXIS2_PLACEMENT_3D ( 'NONE', #1864, #1600, #9714 ) ;
#5075 = FACE_OUTER_BOUND ( 'NONE', #4080, .T. ) ;
#5076 = CARTESIAN_POINT ( 'NONE',  ( 122.2593324768346008, 19.00000000000000000, 173.7755348299889988 ) ) ;
#5077 = CONICAL_SURFACE ( 'NONE', #7213, 6.500000000000005329, 0.7853981633974476129 ) ;
#5078 = ADVANCED_FACE ( 'NONE', ( #826 ), #11265, .T. ) ;
#5079 = AXIS2_PLACEMENT_3D ( 'NONE', #159, #1158, #4347 ) ;
#5080 = ADVANCED_FACE ( 'NONE', ( #6960 ), #2728, .T. ) ;
#5081 = CONICAL_SURFACE ( 'NONE', #8708, 6.500000000000000000, 0.7853981633974518317 ) ;
#5082 = CARTESIAN_POINT ( 'NONE',  ( -259.4723857429225404, 19.96883746178179209, 34.18476129330913693 ) ) ;
#5083 = CARTESIAN_POINT ( 'NONE',  ( -239.4571233178585317, -1.786328300567973315, -11.86629109653343050 ) ) ;
#5084 = DIRECTION ( 'NONE',  ( 0.000000000000000000, 0.000000000000000000, 1.000000000000000000 ) ) ;
#5085 = CARTESIAN_POINT ( 'NONE',  ( -245.4148443365517949, 8.946846751025407940, 7.616852152958314193 ) ) ;
#5086 = ADVANCED_FACE ( 'NONE', ( #4888 ), #8024, .F. ) ;
#5087 = AXIS2_PLACEMENT_3D ( 'NONE', #7643, #7834, #11909 ) ;
#5088 = EDGE_LOOP ( 'NONE', ( #1938, #5743, #5688, #6764 ) ) ;
#5089 = DIRECTION ( 'NONE',  ( 0.000000000000000000, -1.000000000000000000, 0.000000000000000000 ) ) ;
#5090 = ORIENTED_EDGE ( 'NONE', *, *, #6885, .T. ) ;
#5091 = LINE ( 'NONE', #43, #9063 ) ;
#5092 = ORIENTED_EDGE ( 'NONE', *, *, #5835, .T. ) ;
#5093 = TOROIDAL_SURFACE ( 'NONE', #3181, 250.0000000000000000, 10.00000000000000000 ) ;
#5094 = CARTESIAN_POINT ( 'NONE',  ( 131.7449682071765835, -18.00000000000000000, -261.2053404739389180 ) ) ;
#5095 = EDGE_CURVE ( 'NONE', #5893, #10423, #12155, .T. ) ;
#5096 = CARTESIAN_POINT ( 'NONE',  ( 240.2193860686244022, 2.381856054652649934, 2.564741263481397304 ) ) ;
#5097 = DIRECTION ( 'NONE',  ( 8.659560562354951347E-17, -0.7071067811865460184, 0.7071067811865489050 ) ) ;
#5098 = CARTESIAN_POINT ( 'NONE',  ( 220.9845196385168435, -30.00000000000000000, -190.9766794143566528 ) ) ;
#5099 = AXIS2_PLACEMENT_3D ( 'NONE', #6655, #387, #1583 ) ;
#5100 = DIRECTION ( 'NONE',  ( 1.000000000000000000, 0.000000000000000000, -1.224646799147353207E-16 ) ) ;
#5101 = CARTESIAN_POINT ( 'NONE',  ( 122.2593324768334071, 30.00000000000000000, -168.2755348299895104 ) ) ;
#5102 = CARTESIAN_POINT ( 'NONE',  ( -257.4287020129719963, 20.79694577634646180, 42.50473797389691555 ) ) ;
#5103 = CONTEXT_DEPENDENT_SHAPE_REPRESENTATION ( #7782, #1677 ) ;
#5104 = EDGE_LOOP ( 'NONE', ( #4194, #11843 ) ) ;
#5105 = CARTESIAN_POINT ( 'NONE',  ( -238.7118990657748157, -0.07233802403633284028, -11.74979657428336211 ) ) ;
#5106 = VERTEX_POINT ( 'NONE', #10087 ) ;
#5107 = CARTESIAN_POINT ( 'NONE',  ( -249.2714863791366611, 10.50505558484134738, -5.263680432602310333 ) ) ;
#5108 = CARTESIAN_POINT ( 'NONE',  ( -246.2818250957594159, -9.328552628636005650, -7.548386157348565995 ) ) ;
#5109 = AXIS2_PLACEMENT_3D ( 'NONE', #2122, #9127, #3989 ) ;
#5110 = DIRECTION ( 'NONE',  ( 0.7823834078220653909, 0.5538822189107470706, -0.2847642722309787766 ) ) ;
#5111 = CARTESIAN_POINT ( 'NONE',  ( -249.0239419977331750, -10.26696504969905277, 5.714577089209429417 ) ) ;
#5112 = ORIENTED_EDGE ( 'NONE', *, *, #9814, .F. ) ;
#5113 = CARTESIAN_POINT ( 'NONE',  ( -247.4557548097905055, 20.79694577642381859, 84.02568524162670371 ) ) ;
#5114 = DIRECTION ( 'NONE',  ( 0.6368676505102695007, 0.000000000000000000, 0.7709731485165545184 ) ) ;
#5115 = DIRECTION ( 'NONE',  ( 0.000000000000000000, 0.000000000000000000, 1.000000000000000000 ) ) ;
#5116 = AXIS2_PLACEMENT_3D ( 'NONE', #2214, #6289, #10341 ) ;
#5117 = CARTESIAN_POINT ( 'NONE',  ( -244.2656328536486967, -8.290010951899001057, -8.326962424612901259 ) ) ;
#5118 = PRODUCT_DEFINITION_FORMATION_WITH_SPECIFIED_SOURCE ( 'ANY', '', #8315, .NOT_KNOWN. ) ;
#5119 = DIRECTION ( 'NONE',  ( 0.7210484489137145570, 0.5538822189107472926, 0.4162975160791064777 ) ) ;
#5120 = CARTESIAN_POINT ( 'NONE',  ( -229.7045047833707940, -1.539767244506014432, 11.65512487062059677 ) ) ;
#5121 = CARTESIAN_POINT ( 'NONE',  ( -23.54981712579611042, -18.00000000000000000, 295.6955080056604288 ) ) ;
#5122 = ORIENTED_EDGE ( 'NONE', *, *, #4273, .F. ) ;
#5123 = ORIENTED_EDGE ( 'NONE', *, *, #4433, .F. ) ;
#5124 = VECTOR ( 'NONE', #3509, 1000.000000000000000 ) ;
#5125 = DIRECTION ( 'NONE',  ( 0.000000000000000000, 0.000000000000000000, -1.000000000000000000 ) ) ;
#5126 = CARTESIAN_POINT ( 'NONE',  ( 130.5770120857756069, 20.08915143320244567, -226.1171533158560010 ) ) ;
#5127 = DIRECTION ( 'NONE',  ( -0.000000000000000000, 0.8560027256360644987, -0.5169713083949903920 ) ) ;
#5128 = EDGE_CURVE ( 'NONE', #5475, #6733, #3374, .T. ) ;
#5129 = EDGE_CURVE ( 'NONE', #644, #8290, #2876, .T. ) ;
#5130 = DIRECTION ( 'NONE',  ( 0.000000000000000000, 1.000000000000000000, 0.000000000000000000 ) ) ;
#5131 = DIRECTION ( 'NONE',  ( 0.000000000000000000, 0.000000000000000000, 1.000000000000000000 ) ) ;
#5132 = CARTESIAN_POINT ( 'NONE',  ( 159.0697709852749995, 20.79694577591498472, -207.3438552938715134 ) ) ;
#5133 = CIRCLE ( 'NONE', #2785, 305.0000000000000000 ) ;
#5134 = DIRECTION ( 'NONE',  ( 0.6368676505102706109, 0.000000000000000000, 0.7709731485165535192 ) ) ;
#5135 = CARTESIAN_POINT ( 'NONE',  ( 0.000000000000000000, 0.000000000000000000, 0.000000000000000000 ) ) ;
#5136 = CARTESIAN_POINT ( 'NONE',  ( -243.1363860133195089, -7.429686608487776844, 9.102873391554766158 ) ) ;
#5137 = CARTESIAN_POINT ( 'NONE',  ( -245.3462090940810754, 8.922924800614550733, 8.026147510179294287 ) ) ;
#5138 = ORIENTED_EDGE ( 'NONE', *, *, #14, .F. ) ;
#5139 = PRODUCT_DEFINITION ( 'UNKNOWN', '', #5118, #2875 ) ;
#5140 = CONICAL_SURFACE ( 'NONE', #2792, 6.500000000000005329, 0.7853981633974518317 ) ;
#5141 = CARTESIAN_POINT ( 'NONE',  ( 0.000000000000000000, 19.00000000000000000, 213.5000000000000000 ) ) ;
#5142 = CARTESIAN_POINT ( 'NONE',  ( 229.9884266870191709, -2.636753545538539800, 2.312936221645658819 ) ) ;
#5143 = ORIENTED_EDGE ( 'NONE', *, *, #4031, .F. ) ;
#5144 = ORIENTED_EDGE ( 'NONE', *, *, #4273, .T. ) ;
#5145 = DIRECTION ( 'NONE',  ( 0.6368676505102689456, 0.000000000000000000, 0.7709731485165549625 ) ) ;
#5146 = ORIENTED_EDGE ( 'NONE', *, *, #10265, .T. ) ;
#5147 = CARTESIAN_POINT ( 'NONE',  ( -17.09264059789343193, 19.96883746059643983, -261.1558126970361400 ) ) ;
#5148 = LINE ( 'NONE', #12033, #11769 ) ;
#5149 = DIRECTION ( 'NONE',  ( 0.000000000000000000, 0.000000000000000000, 1.000000000000000000 ) ) ;
#5150 = AXIS2_PLACEMENT_3D ( 'NONE', #4686, #10763, #10964 ) ;
#5151 = CARTESIAN_POINT ( 'NONE',  ( -241.3664650619784311, 5.412961098280363537, 10.42892899847316102 ) ) ;
#5152 = ORIENTED_EDGE ( 'NONE', *, *, #10380, .T. ) ;
#5153 = CARTESIAN_POINT ( 'NONE',  ( 137.7829567244532143, 20.79694577634646180, 221.5672498511019626 ) ) ;
#5154 = EDGE_CURVE ( 'NONE', #7072, #6121, #1891, .T. ) ;
#5155 = ORIENTED_EDGE ( 'NONE', *, *, #6073, .T. ) ;
#5156 = EDGE_CURVE ( 'NONE', #11433, #11239, #7854, .T. ) ;
#5157 = DIRECTION ( 'NONE',  ( 0.000000000000000000, -1.000000000000000000, 0.000000000000000000 ) ) ;
#5158 = ORIENTED_EDGE ( 'NONE', *, *, #1439, .F. ) ;
#5159 = VECTOR ( 'NONE', #10555, 1000.000000000000000 ) ;
#5160 = AXIS2_PLACEMENT_3D ( 'NONE', #2435, #571, #318 ) ;
#5161 = DIRECTION ( 'NONE',  ( 1.000000000000000000, 0.000000000000000000, 0.000000000000000000 ) ) ;
#5162 = CARTESIAN_POINT ( 'NONE',  ( 239.2711857406566764, 1.179132569667092456, 3.296284915102607904 ) ) ;
#5163 = CARTESIAN_POINT ( 'NONE',  ( 286.5445428119865596, -18.00000000000000000, 22.67813138875427370 ) ) ;
#5164 = DIRECTION ( 'NONE',  ( 0.000000000000000000, 1.000000000000000000, 0.000000000000000000 ) ) ;
#5165 = PRODUCT_DEFINITION_SHAPE ( 'NONE', 'NONE',  #13113 ) ;
#5166 = DIRECTION ( 'NONE',  ( -0.000000000000000000, -1.000000000000000000, 0.000000000000000000 ) ) ;
#5167 = AXIS2_PLACEMENT_3D ( 'NONE', #4335, #2268, #1278 ) ;
#5168 = CARTESIAN_POINT ( 'NONE',  ( -252.0229195836994336, 20.79694577634646535, 67.53249125288826349 ) ) ;
#5169 = EDGE_LOOP ( 'NONE', ( #3120, #10604, #6664, #10049 ) ) ;
#5170 = CIRCLE ( 'NONE', #10716, 6.500000000000005329 ) ;
#5171 = DIRECTION ( 'NONE',  ( 0.000000000000000000, 0.000000000000000000, 1.000000000000000000 ) ) ;
#5172 = ORIENTED_EDGE ( 'NONE', *, *, #7902, .T. ) ;
#5173 = EDGE_CURVE ( 'NONE', #3688, #3038, #9759, .T. ) ;
#5174 = CARTESIAN_POINT ( 'NONE',  ( 122.2593324768334071, 30.00000000000000000, -173.7755348299895104 ) ) ;
#5175 = CARTESIAN_POINT ( 'NONE',  ( -243.1855895750504430, -7.483404893957491311, -9.380758043683870895 ) ) ;
#5176 = CARTESIAN_POINT ( 'NONE',  ( -249.7266004377088393, -11.33448610411373991, 3.100135290851260272 ) ) ;
#5177 = ORIENTED_EDGE ( 'NONE', *, *, #4393, .T. ) ;
#5178 = AXIS2_PLACEMENT_3D ( 'NONE', #5844, #3895, #1840 ) ;
#5179 = EDGE_CURVE ( 'NONE', #7165, #10853, #4950, .T. ) ;
#5180 = CARTESIAN_POINT ( 'NONE',  ( -196.4640694359484883, 20.79694577636040265, -172.3268284091419957 ) ) ;
#5181 = CARTESIAN_POINT ( 'NONE',  ( -240.7937243741888551, 4.465328606765308628, -11.13898957095615572 ) ) ;
#5182 = CARTESIAN_POINT ( 'NONE',  ( -239.5361044668155159, 1.848645179572584896, 11.60366368868220022 ) ) ;
#5183 = CARTESIAN_POINT ( 'NONE',  ( -245.4623802705897333, -8.970018889905636783, -7.589566413994238481 ) ) ;
#5184 =( REPRESENTATION_RELATIONSHIP ('NONE','NONE', #12019, #5191 ) REPRESENTATION_RELATIONSHIP_WITH_TRANSFORMATION ( #10324 )SHAPE_REPRESENTATION_RELATIONSHIP( ) );
#5185 = CARTESIAN_POINT ( 'NONE',  ( 239.4068548683480628, -1.402387639798359231, 3.207804078318175378 ) ) ;
#5186 = DIRECTION ( 'NONE',  ( 0.8042250444015763833, 0.5538822189107471816, 0.2154914511802957233 ) ) ;
#5187 = B_SPLINE_CURVE_WITH_KNOTS ( 'NONE', 3,
 ( #2447, #1324, #4504, #258, #12708, #11593, #7582, #7520, #9458, #9391, #1257, #10520, #6329, #10379, #8590, #2508, #7326, #3510, #8464, #7454, #12518, #12648, #10646, #9514, #6525, #6590, #2384, #9636, #523, #5321, #4569, #4315, #8652, #12458, #5452, #3311, #10453, #5390, #7389, #330 ),
 .UNSPECIFIED., .F., .F.,
 ( 4, 2, 1, 1, 2, 2, 2, 2, 1, 1, 2, 2, 2, 2, 1, 1, 1, 1, 2, 2, 2, 2, 2, 4 ),
 ( 0.5002288818359376110, 0.5627002716060051091, 0.5939359664910388581, 0.6095538139335572314, 0.6173627376548146417, 0.6251716613760720520, 0.6876430511461220085, 0.7188787460311498734, 0.7344965934736605861, 0.7423055171949158870, 0.7462099790555436485, 0.7501144409161712989, 0.8125858306861062363, 0.8438215255710737051, 0.8594393730135573284, 0.8672482967347945326, 0.8711527585954177422, 0.8731049895257294580, 0.8740811049908898678, 0.8750572204560502776, 0.9062929153420298256, 0.9219107627850194886, 0.9375286102280091516, 1.000000000000000000 ),
 .UNSPECIFIED. ) ;
#5188 = CARTESIAN_POINT ( 'NONE',  ( -229.9710174714563209, 11.43162843135961459, -3.668625443667830499 ) ) ;
#5189 = AXIS2_PLACEMENT_3D ( 'NONE', #1274, #12473, #3324 ) ;
#5190 = CONTEXT_DEPENDENT_SHAPE_REPRESENTATION ( #12883, #11869 ) ;
#5191 = SHAPE_REPRESENTATION ( 'Ball Separator Polymer', ( #805 ), #9955 ) ;
#5192 = DIRECTION ( 'NONE',  ( -0.6368676505102737195, 0.000000000000000000, -0.7709731485165509657 ) ) ;
#5193 = ORIENTED_EDGE ( 'NONE', *, *, #956, .T. ) ;
#5194 = CIRCLE ( 'NONE', #6914, 6.500000000000005329 ) ;
#5195 = ORIENTED_EDGE ( 'NONE', *, *, #708, .F. ) ;
#5196 = CARTESIAN_POINT ( 'NONE',  ( -226.1171533167550081, 20.08915143289658545, -130.5770120871825952 ) ) ;
#5197 = LINE ( 'NONE', #12071, #7579 ) ;
#5198 = PRODUCT_DEFINITION_SHAPE ( 'NONE', 'NONE',  #13096 ) ;
#5199 = VECTOR ( 'NONE', #6343, 1000.000000000000000 ) ;
#5200 = CARTESIAN_POINT ( 'NONE',  ( 3.012631125902489062E-14, 23.50000000000000000, 246.0000000000000000 ) ) ;
#5201 = AXIS2_PLACEMENT_3D ( 'NONE', #4636, #3517, #12779 ) ;
#5202 = CARTESIAN_POINT ( 'NONE',  ( 0.000000000000000000, 0.000000000000000000, -249.7999999999999829 ) ) ;
#5203 = CARTESIAN_POINT ( 'NONE',  ( 71.82423009839129691, 18.00000000000000000, -190.8354503650405150 ) ) ;
#5204 = DIRECTION ( 'NONE',  ( 0.000000000000000000, -1.000000000000000000, 0.000000000000000000 ) ) ;
#5205 = CARTESIAN_POINT ( 'NONE',  ( 0.000000000000000000, 0.000000000000000000, 0.000000000000000000 ) ) ;
#5206 = DIRECTION ( 'NONE',  ( -0.5363228529974879422, -0.1961161351381840445, 0.8209118459926720845 ) ) ;
#5207 = VERTEX_POINT ( 'NONE', #8135 ) ;
#5208 = CARTESIAN_POINT ( 'NONE',  ( 197.8197553893920144, 18.00000000000000000, 64.27553482998850143 ) ) ;
#5209 = EDGE_CURVE ( 'NONE', #2022, #8050, #1260, .T. ) ;
#5210 = CIRCLE ( 'NONE', #125, 5.100000000000017408 ) ;
#5211 = PRODUCT_DEFINITION_SHAPE ( 'NONE', 'NONE',  #13043 ) ;
#5212 = CARTESIAN_POINT ( 'NONE',  ( 229.9948716278398706, -3.146202118422226413, 1.550284843520935762 ) ) ;
#5213 = ORIENTED_EDGE ( 'NONE', *, *, #10627, .T. ) ;
#5214 = VERTEX_POINT ( 'NONE', #5017 ) ;
#5215 = FACE_OUTER_BOUND ( 'NONE', #8257, .T. ) ;
#5216 = LINE ( 'NONE', #9290, #4858 ) ;
#5217 = CARTESIAN_POINT ( 'NONE',  ( 207.1687172302655142, 20.08915143321463503, -158.9353507248590063 ) ) ;
#5218 = CONICAL_SURFACE ( 'NONE', #9282, 5.100000000000000533, 0.7853981633974503884 ) ;
#5219 = CARTESIAN_POINT ( 'NONE',  ( 159.3442861576696998, -29.00000000000000000, 192.8974817588416784 ) ) ;
#5220 = DIRECTION ( 'NONE',  ( 0.000000000000000000, 0.000000000000000000, 1.000000000000000000 ) ) ;
#5221 = CIRCLE ( 'NONE', #6935, 6.500000000000005329 ) ;
#5222 = CARTESIAN_POINT ( 'NONE',  ( -246.9758887651909163, 9.561393940552608939, 6.829510940766356342 ) ) ;
#5223 = ORIENTED_EDGE ( 'NONE', *, *, #12085, .T. ) ;
#5224 = DIRECTION ( 'NONE',  ( 0.000000000000000000, 0.000000000000000000, 1.000000000000000000 ) ) ;
#5225 = EDGE_CURVE ( 'NONE', #1921, #8685, #10146, .T. ) ;
#5226 = VERTEX_POINT ( 'NONE', #6028 ) ;
#5227 = DIRECTION ( 'NONE',  ( -0.4503334343941563511, -0.7071067811865480168, -0.5451603414287977678 ) ) ;
#5228 = ORIENTED_EDGE ( 'NONE', *, *, #7989, .F. ) ;
#5229 = ORIENTED_EDGE ( 'NONE', *, *, #7578, .T. ) ;
#5230 = AXIS2_PLACEMENT_3D ( 'NONE', #11414, #10337, #410 ) ;
#5231 =( REPRESENTATION_RELATIONSHIP ('NONE','NONE', #12019, #182 ) REPRESENTATION_RELATIONSHIP_WITH_TRANSFORMATION ( #3911 )SHAPE_REPRESENTATION_RELATIONSHIP( ) );
#5232 = CIRCLE ( 'NONE', #9918, 5.500000000000005329 ) ;
#5233 = CARTESIAN_POINT ( 'NONE',  ( 159.9811538081799540, 20.00000000000000000, 193.6684549073582673 ) ) ;
#5234 = DIRECTION ( 'NONE',  ( 0.000000000000000000, 1.000000000000000000, 0.000000000000000000 ) ) ;
#5235 = FACE_OUTER_BOUND ( 'NONE', #7847, .T. ) ;
#5236 = EDGE_CURVE ( 'NONE', #12366, #12887, #9554, .T. ) ;
#5237 = DIRECTION ( 'NONE',  ( 0.000000000000000000, -1.000000000000000000, 0.000000000000000000 ) ) ;
#5238 = ADVANCED_FACE ( 'NONE', ( #5075 ), #8703, .T. ) ;
#5239 = DIRECTION ( 'NONE',  ( 0.6368676505102700558, 0.000000000000000000, 0.7709731485165541853 ) ) ;
#5240 = DIRECTION ( 'NONE',  ( 0.6368676505102716101, 0.000000000000000000, 0.7709731485165527420 ) ) ;
#5241 = ITEM_DEFINED_TRANSFORMATION ( 'NONE', 'NONE', #3573,  #805 ) ;
#5242 = ORIENTED_EDGE ( 'NONE', *, *, #135, .F. ) ;
#5243 = FACE_BOUND ( 'NONE', #364, .T. ) ;
#5244 = ORIENTED_EDGE ( 'NONE', *, *, #278, .T. ) ;
#5245 = DIRECTION ( 'NONE',  ( 0.000000000000000000, -0.1961161351381850160, -0.9805806756909200006 ) ) ;
#5246 = DIRECTION ( 'NONE',  ( 0.000000000000000000, 0.000000000000000000, 1.000000000000000000 ) ) ;
#5247 =( REPRESENTATION_RELATIONSHIP ('NONE','NONE', #12019, #182 ) REPRESENTATION_RELATIONSHIP_WITH_TRANSFORMATION ( #4620 )SHAPE_REPRESENTATION_RELATIONSHIP( ) );
#5248 = CARTESIAN_POINT ( 'NONE',  ( -249.7845036514944468, -11.60839712336035845, 1.818694302480377889 ) ) ;
#5249 = EDGE_LOOP ( 'NONE', ( #10152, #4694, #2749, #4611 ) ) ;
#5250 = CARTESIAN_POINT ( 'NONE',  ( -260.7745447066434963, 20.79694577614318618, -17.06760680913714978 ) ) ;
#5251 = CARTESIAN_POINT ( 'NONE',  ( -241.3126941818516400, 5.350247869163432313, -10.74127079069710788 ) ) ;
#5252 = DIRECTION ( 'NONE',  ( 0.000000000000000000, 0.000000000000000000, -1.000000000000000000 ) ) ;
#5253 =( REPRESENTATION_RELATIONSHIP ('NONE','NONE', #12019, #11156 ) REPRESENTATION_RELATIONSHIP_WITH_TRANSFORMATION ( #1591 )SHAPE_REPRESENTATION_RELATIONSHIP( ) );
#5254 = EDGE_CURVE ( 'NONE', #7121, #10886, #3367, .T. ) ;
#5255 = CARTESIAN_POINT ( 'NONE',  ( -242.2371604626287649, -6.538578786747162752, -9.762666687019821765 ) ) ;
#5256 = EDGE_CURVE ( 'NONE', #9399, #6766, #7228, .T. ) ;
#5257 = CARTESIAN_POINT ( 'NONE',  ( 238.9743709119342441, -0.1785824616379369512, 3.500006748982332994 ) ) ;
#5258 = DIRECTION ( 'NONE',  ( 0.6378047977532466106, 0.5538822189107470706, 0.5351817705578614248 ) ) ;
#5259 = CARTESIAN_POINT ( 'NONE',  ( 240.5832516929813494, 3.370511182575330000, -0.9484507949093432533 ) ) ;
#5260 = EDGE_CURVE ( 'NONE', #11029, #9991, #2945, .T. ) ;
#5261 = DIRECTION ( 'NONE',  ( 0.000000000000000000, 1.000000000000000000, 0.000000000000000000 ) ) ;
#5262 = ORIENTED_EDGE ( 'NONE', *, *, #6118, .F. ) ;
#5263 = AXIS2_PLACEMENT_3D ( 'NONE', #7726, #3924, #7998 ) ;
#5264 = CARTESIAN_POINT ( 'NONE',  ( -1.009475258464312158E-12, 20.08915143297736350, 260.5542428351129729 ) ) ;
#5265 = CARTESIAN_POINT ( 'NONE',  ( 227.3999999999999773, 2.999417280921144346, -0.05912676983912699968 ) ) ;
#5266 = CARTESIAN_POINT ( 'NONE',  ( -249.6767732310727865, 11.18100465983052949, 3.612153022792313095 ) ) ;
#5267 = LINE ( 'NONE', #9338, #6176 ) ;
#5268 = ADVANCED_FACE ( 'NONE', ( #2350 ), #6228, .F. ) ;
#5269 = DIRECTION ( 'NONE',  ( -0.000000000000000000, 0.8560027256360644987, -0.5169713083949903920 ) ) ;
#5270 = CARTESIAN_POINT ( 'NONE',  ( -247.9529057712887834, -9.807895051005736775, 6.914131050820655489 ) ) ;
#5271 = DIRECTION ( 'NONE',  ( 0.6368676505102698338, 0.000000000000000000, 0.7709731485165541853 ) ) ;
#5272 = DIRECTION ( 'NONE',  ( 0.8191520442889986819, 0.000000000000000000, -0.5735764363510362784 ) ) ;
#5273 = CARTESIAN_POINT ( 'NONE',  ( -246.4294064422139741, -9.379184893293130543, 7.077828147970874006 ) ) ;
#5274 = ITEM_DEFINED_TRANSFORMATION ( 'NONE', 'NONE', #2301,  #805 ) ;
#5275 = ORIENTED_EDGE ( 'NONE', *, *, #9525, .F. ) ;
#5276 = CARTESIAN_POINT ( 'NONE',  ( 71.82423009839129691, 19.40000000000000213, -197.3354503650404865 ) ) ;
#5277 = DIRECTION ( 'NONE',  ( 0.000000000000000000, 1.000000000000000000, 0.000000000000000000 ) ) ;
#5278 = ORIENTED_EDGE ( 'NONE', *, *, #12634, .F. ) ;
#5279 = ORIENTED_EDGE ( 'NONE', *, *, #92, .F. ) ;
#5280 = FACE_OUTER_BOUND ( 'NONE', #10273, .T. ) ;
#5281 = CARTESIAN_POINT ( 'NONE',  ( -27.68945685411286561, -19.00000000000000000, 290.6841825403027997 ) ) ;
#5282 = AXIS2_PLACEMENT_3D ( 'NONE', #12879, #7877, #11949 ) ;
#5283 = CARTESIAN_POINT ( 'NONE',  ( 172.5787240287722284, 19.96883746003332405, -196.7513681799441656 ) ) ;
#5284 = CARTESIAN_POINT ( 'NONE',  ( 0.000000000000000000, 22.00000000000000000, 250.7029414592220178 ) ) ;
#5285 = DIRECTION ( 'NONE',  ( -0.7071067811865487940, 0.000000000000000000, 0.7071067811865463515 ) ) ;
#5286 = CARTESIAN_POINT ( 'NONE',  ( 0.000000000000000000, -22.00000000000000000, 0.000000000000000000 ) ) ;
#5287 = EDGE_LOOP ( 'NONE', ( #3631, #12717, #9932, #8376 ) ) ;
#5288 = AXIS2_PLACEMENT_3D ( 'NONE', #10485, #421, #224 ) ;
#5289 = CIRCLE ( 'NONE', #6577, 249.7999999999999829 ) ;
#5290 = CARTESIAN_POINT ( 'NONE',  ( 115.4021059068215607, 20.79694577634647246, 234.0054343868620208 ) ) ;
#5291 = EDGE_LOOP ( 'NONE', ( #183, #12677, #7499, #2581 ) ) ;
#5292 = CIRCLE ( 'NONE', #3797, 240.3921568627449687 ) ;
#5293 = FACE_OUTER_BOUND ( 'NONE', #8, .T. ) ;
#5294 = ORIENTED_EDGE ( 'NONE', *, *, #12898, .F. ) ;
#5295 = ORIENTED_EDGE ( 'NONE', *, *, #1933, .F. ) ;
#5296 = VECTOR ( 'NONE', #3953, 999.9999999999998863 ) ;
#5297 = VECTOR ( 'NONE', #5795, 1000.000000000000000 ) ;
#5298 = LINE ( 'NONE', #2493, #927 ) ;
#5299 = DIRECTION ( 'NONE',  ( 0.000000000000000000, -0.8560027256360642767, 0.5169713083949908361 ) ) ;
#5300 = DIRECTION ( 'NONE',  ( -0.000000000000000000, -1.000000000000000000, 0.000000000000000000 ) ) ;
#5301 = ADVANCED_FACE ( 'NONE', ( #5280 ), #5724, .F. ) ;
#5302 = EDGE_CURVE ( 'NONE', #5843, #11287, #3586, .T. ) ;
#5303 = CARTESIAN_POINT ( 'NONE',  ( 227.3999999999999773, 0.000000000000000000, 0.000000000000000000 ) ) ;
#5304 = VECTOR ( 'NONE', #7374, 1000.000000000000000 ) ;
#5305 = CARTESIAN_POINT ( 'NONE',  ( -197.8197553893909912, 30.00000000000000000, 64.27553482999130097 ) ) ;
#5306 = CARTESIAN_POINT ( 'NONE',  ( -246.7640704956085926, 9.498771479817998298, 7.332983348267928747 ) ) ;
#5307 = CARTESIAN_POINT ( 'NONE',  ( 139.1326329530957082, -28.60000000000000142, -252.2620519511468729 ) ) ;
#5308 = CARTESIAN_POINT ( 'NONE',  ( 233.5975020798683204, 0.000000000000000000, 0.000000000000000000 ) ) ;
#5309 = AXIS2_PLACEMENT_3D ( 'NONE', #4145, #11082, #4006 ) ;
#5310 = ORIENTED_EDGE ( 'NONE', *, *, #3748, .T. ) ;
#5311 = DIRECTION ( 'NONE',  ( 0.000000000000000000, 1.000000000000000000, 0.000000000000000000 ) ) ;
#5312 = ORIENTED_EDGE ( 'NONE', *, *, #2991, .F. ) ;
#5313 = CARTESIAN_POINT ( 'NONE',  ( -248.0831933713610056, 9.830508068705238856, -6.436117704883929314 ) ) ;
#5314 = DIRECTION ( 'NONE',  ( 0.000000000000000000, 0.7071067811865470176, 0.7071067811865480168 ) ) ;
#5315 = AXIS2_PLACEMENT_3D ( 'NONE', #1238, #5300, #4297 ) ;
#5316 = DIRECTION ( 'NONE',  ( 0.000000000000000000, 1.000000000000000000, 0.000000000000000000 ) ) ;
#5317 = ORIENTED_EDGE ( 'NONE', *, *, #4463, .T. ) ;
#5318 = CIRCLE ( 'NONE', #433, 6.500000000000005329 ) ;
#5319 = CARTESIAN_POINT ( 'NONE',  ( 196.4640694362159934, 20.79694577623644491, 172.3268284092819727 ) ) ;
#5320 = CARTESIAN_POINT ( 'NONE',  ( -244.8469727607960351, 8.653369516572549713, -8.313800303827326488 ) ) ;
#5321 = CARTESIAN_POINT ( 'NONE',  ( -239.4273512216421409, 1.756910838264598596, 11.87068934081676019 ) ) ;
#5322 = CARTESIAN_POINT ( 'NONE',  ( -243.2136795283335857, -7.496740008778170150, -9.047741638628279404 ) ) ;
#5323 = CIRCLE ( 'NONE', #9787, 5.500000000000005329 ) ;
#5324 = CARTESIAN_POINT ( 'NONE',  ( 239.3580835733109495, -1.327753754010405851, 3.239279126423496802 ) ) ;
#5325 = PRODUCT_DEFINITION_SHAPE ( 'NONE', 'NONE',  #13073 ) ;
#5326 = CARTESIAN_POINT ( 'NONE',  ( 240.4516407507319400, 2.994726891335696806, 1.822055168078867471 ) ) ;
#5327 = ADVANCED_FACE ( 'NONE', ( #5215 ), #4150, .F. ) ;
#5328 = EDGE_CURVE ( 'NONE', #9350, #6648, #12482, .T. ) ;
#5329 = AXIS2_PLACEMENT_3D ( 'NONE', #9418, #2143, #216 ) ;
#5330 = CARTESIAN_POINT ( 'NONE',  ( -239.9450917581424960, 2.156506209390990136, -11.80463811257499884 ) ) ;
#5331 = VERTEX_POINT ( 'NONE', #8232 ) ;
#5332 = CARTESIAN_POINT ( 'NONE',  ( 247.2466869560049929, 20.08915143286045790, 83.95474316005440585 ) ) ;
#5333 = FACE_BOUND ( 'NONE', #12755, .T. ) ;
#5334 = DIRECTION ( 'NONE',  ( 0.000000000000000000, 0.9998057603070481525, -0.01970892327970899874 ) ) ;
#5335 = CARTESIAN_POINT ( 'NONE',  ( 224.4939760857161843, -2.899436704890439476, 0.05715587751115645126 ) ) ;
#5336 = CARTESIAN_POINT ( 'NONE',  ( 239.3359268379452658, -1.289900281489894995, -3.253812819841678472 ) ) ;
#5337 = AXIS2_PLACEMENT_3D ( 'NONE', #12201, #11193, #4319 ) ;
#5338 = DIRECTION ( 'NONE',  ( 0.000000000000000000, 1.000000000000000000, 0.000000000000000000 ) ) ;
#5339 =( REPRESENTATION_RELATIONSHIP ('NONE','NONE', #12019, #5191 ) REPRESENTATION_RELATIONSHIP_WITH_TRANSFORMATION ( #6 )SHAPE_REPRESENTATION_RELATIONSHIP( ) );
#5340 = CARTESIAN_POINT ( 'NONE',  ( -246.3576883206671653, -9.357104192533332920, 7.512982112701342530 ) ) ;
#5341 = CARTESIAN_POINT ( 'NONE',  ( 227.3999999999999773, -4.447920636657316074, 2.686261716586446635 ) ) ;
#5342 = CARTESIAN_POINT ( 'NONE',  ( -14.31396777367070783, -138.4705547276867321, 39.32730324096132790 ) ) ;
#5343 = DIRECTION ( 'NONE',  ( 0.4503334343941555740, 0.7071067811865490160, 0.5451603414287971017 ) ) ;
#5344 = ORIENTED_EDGE ( 'NONE', *, *, #1742, .T. ) ;
#5345 = DIRECTION ( 'NONE',  ( 0.000000000000000000, 1.000000000000000000, 0.000000000000000000 ) ) ;
#5346 = DIRECTION ( 'NONE',  ( 0.000000000000000000, -1.000000000000000000, 0.000000000000000000 ) ) ;
#5347 = EDGE_CURVE ( 'NONE', #10920, #13016, #3336, .T. ) ;
#5348 = B_SPLINE_CURVE_WITH_KNOTS ( 'NONE', 3,
 ( #10774, #580, #843, #8710, #12839, #10975, #3833, #1846, #11844, #4828, #13039, #12772, #11033 ),
 .UNSPECIFIED., .F., .F.,
 ( 4, 2, 2, 1, 2, 2, 4 ),
 ( 0.000000000000000000, 0.2499999999999983347, 0.3749999999999975020, 0.4374999999999973910, 0.4687499999999859002, 0.4999999999999743538, 1.000000000000000000 ),
 .UNSPECIFIED. ) ;
#5349 = CARTESIAN_POINT ( 'NONE',  ( 229.9750547325863010, -0.9088897890003139191, -3.387654320631149130 ) ) ;
#5350 = ORIENTED_EDGE ( 'NONE', *, *, #5637, .T. ) ;
#5351 = ORIENTED_EDGE ( 'NONE', *, *, #2286, .T. ) ;
#5352 = CARTESIAN_POINT ( 'NONE',  ( -290.6841825403030839, -30.00000000000000000, -27.68945685411394919 ) ) ;
#5353 = DIRECTION ( 'NONE',  ( 0.000000000000000000, 0.000000000000000000, 1.000000000000000000 ) ) ;
#5354 = UNCERTAINTY_MEASURE_WITH_UNIT (LENGTH_MEASURE( 1.000000000000000082E-05 ), #7526, 'distance_accuracy_value', 'NONE');
#5355 = AXIS2_PLACEMENT_3D ( 'NONE', #8313, #4100, #12372 ) ;
#5356 = CARTESIAN_POINT ( 'NONE',  ( 159.3024069666089133, 19.96883745889249795, 207.6469600140662806 ) ) ;
#5357 = FACE_OUTER_BOUND ( 'NONE', #7772, .T. ) ;
#5358 = FACE_OUTER_BOUND ( 'NONE', #131, .T. ) ;
#5359 = DIRECTION ( 'NONE',  ( 0.6427876096865379196, 0.000000000000000000, 0.7660444431189792347 ) ) ;
#5360 = CARTESIAN_POINT ( 'NONE',  ( 225.1241593668336236, -29.00000000000000000, -185.9653539489990521 ) ) ;
#5361 = ORIENTED_EDGE ( 'NONE', *, *, #6936, .T. ) ;
#5362 = CARTESIAN_POINT ( 'NONE',  ( 67.53249125288894561, 20.79694577634646180, 252.0229195836991494 ) ) ;
#5363 = ORIENTED_EDGE ( 'NONE', *, *, #9006, .F. ) ;
#5364 = CARTESIAN_POINT ( 'NONE',  ( -229.2637990951503753, -30.00000000000000000, 180.9540284836414514 ) ) ;
#5365 = ORIENTED_EDGE ( 'NONE', *, *, #9538, .F. ) ;
#5366 = VERTEX_POINT ( 'NONE', #2148 ) ;
#5367 = AXIS2_PLACEMENT_3D ( 'NONE', #11739, #1470, #1663 ) ;
#5368 = DIRECTION ( 'NONE',  ( -0.000000000000000000, -1.000000000000000000, 0.000000000000000000 ) ) ;
#5369 = CARTESIAN_POINT ( 'NONE',  ( -122.2593324768359935, 30.00000000000000000, -168.2755348299880040 ) ) ;
#5370 = CARTESIAN_POINT ( 'NONE',  ( -0.000000000000000000, -30.00000000000000000, 0.000000000000000000 ) ) ;
#5371 = CARTESIAN_POINT ( 'NONE',  ( 239.6582758818212540, 1.713542963916843131, -3.052483991371184757 ) ) ;
#5372 = CARTESIAN_POINT ( 'NONE',  ( -122.2593324768359935, 19.00000000000000000, -168.2755348299880040 ) ) ;
#5373 = CARTESIAN_POINT ( 'NONE',  ( -242.2842939341516626, 6.604577240802537830, 10.01896504304081326 ) ) ;
#5374 = CARTESIAN_POINT ( 'NONE',  ( 153.9282213272189495, -30.00000000000000000, 245.7765299597151341 ) ) ;
#5375 = CONICAL_SURFACE ( 'NONE', #4724, 5.099999999999993427, 0.7853981633974461696 ) ;
#5376 = ITEM_DEFINED_TRANSFORMATION ( 'NONE', 'NONE', #8272,  #805 ) ;
#5377 = ORIENTED_EDGE ( 'NONE', *, *, #11829, .F. ) ;
#5378 = CARTESIAN_POINT ( 'NONE',  ( 135.8846079354933352, -19.40000000000000213, -256.1940150085812888 ) ) ;
#5379 = TOROIDAL_SURFACE ( 'NONE', #7712, 238.4705882352940307, 2.000000000000000000 ) ;
#5380 = EDGE_LOOP ( 'NONE', ( #5856, #10846, #2347, #11635 ) ) ;
#5381 = CIRCLE ( 'NONE', #4717, 9.900000000000002132 ) ;
#5382 = CARTESIAN_POINT ( 'NONE',  ( -225.1241593668336236, -19.00000000000000000, 185.9653539489990521 ) ) ;
#5383 = DIRECTION ( 'NONE',  ( 0.000000000000000000, -1.000000000000000000, 0.000000000000000000 ) ) ;
#5384 = EDGE_CURVE ( 'NONE', #9508, #7035, #8504, .T. ) ;
#5385 = EDGE_CURVE ( 'NONE', #4744, #9610, #4223, .T. ) ;
#5386 = CARTESIAN_POINT ( 'NONE',  ( 171.8850263962756628, 20.08915143297737416, -196.0019244007918644 ) ) ;
#5387 = EDGE_LOOP ( 'NONE', ( #7812, #1219, #2213, #1544 ) ) ;
#5388 = DIRECTION ( 'NONE',  ( 1.000000000000000000, 0.000000000000000000, 0.000000000000000000 ) ) ;
#5389 = CARTESIAN_POINT ( 'NONE',  ( -241.3214569866001398, 5.363580936733816529, -10.73461844913050101 ) ) ;
#5390 = CARTESIAN_POINT ( 'NONE',  ( -239.7865846207793936, 2.059993156293506544, 11.82215868828261129 ) ) ;
#5391 = AXIS2_PLACEMENT_3D ( 'NONE', #8222, #12145, #5134 ) ;
#5392 = CARTESIAN_POINT ( 'NONE',  ( 0.000000000000000000, 25.00000000000000000, -245.7999999999999829 ) ) ;
#5393 = AXIS2_PLACEMENT_3D ( 'NONE', #833, #4690, #9960 ) ;
#5394 = PRODUCT_CONTEXT ( 'NONE', #5679, 'mechanical' ) ;
#5395 = DIRECTION ( 'NONE',  ( 0.7709731485165535192, 0.000000000000000000, -0.6368676505102707219 ) ) ;
#5396 = AXIS2_PLACEMENT_3D ( 'NONE', #6637, #6768, #8962 ) ;
#5397 = CIRCLE ( 'NONE', #4961, 249.7999999999999829 ) ;
#5398 = CARTESIAN_POINT ( 'NONE',  ( 122.2593324768346008, 19.00000000000000000, 168.2755348299889988 ) ) ;
#5399 = AXIS2_PLACEMENT_3D ( 'NONE', #3744, #11824, #10681 ) ;
#5400 = EDGE_LOOP ( 'NONE', ( #8773, #4162 ) ) ;
#5401 = CARTESIAN_POINT ( 'NONE',  ( 252.8031682264636117, 19.96883746172993668, -67.71318189737802129 ) ) ;
#5402 = DIRECTION ( 'NONE',  ( -0.000000000000000000, -1.000000000000000000, 0.000000000000000000 ) ) ;
#5403 = FACE_OUTER_BOUND ( 'NONE', #6353, .T. ) ;
#5404 = DIRECTION ( 'NONE',  ( 0.000000000000000000, 0.8757116489157734662, 0.4828344519120573719 ) ) ;
#5405 = DIRECTION ( 'NONE',  ( 0.6368676505102716101, 0.000000000000000000, 0.7709731485165527420 ) ) ;
#5406 = ADVANCED_FACE ( 'NONE', ( #4084 ), #6297, .F. ) ;
#5407 = AXIS2_PLACEMENT_3D ( 'NONE', #11297, #5089, #4290 ) ;
#5408 = ADVANCED_FACE ( 'NONE', ( #223 ), #7413, .F. ) ;
#5409 = DIRECTION ( 'NONE',  ( 0.000000000000000000, 0.000000000000000000, -1.000000000000000000 ) ) ;
#5410 = DIRECTION ( 'NONE',  ( -0.8042250444015778266, 0.5538822189107471816, -0.2154914511802900889 ) ) ;
#5411 = CIRCLE ( 'NONE', #4760, 250.7000000000000171 ) ;
#5412 = DIRECTION ( 'NONE',  ( 0.000000000000000000, 0.000000000000000000, 1.000000000000000000 ) ) ;
#5413 = ITEM_DEFINED_TRANSFORMATION ( 'NONE', 'NONE', #181,  #805 ) ;
#5414 = ORIENTED_EDGE ( 'NONE', *, *, #1363, .F. ) ;
#5415 = CARTESIAN_POINT ( 'NONE',  ( 240.6325187087389565, -3.500040777417273041, 0.1929172344771862835 ) ) ;
#5416 = CARTESIAN_POINT ( 'NONE',  ( -229.9448021440930461, -10.89127638036671719, 5.041528041963096562 ) ) ;
#5417 = EDGE_LOOP ( 'NONE', ( #10849, #11876, #8191, #1792 ) ) ;
#5418 = EDGE_LOOP ( 'NONE', ( #577, #1027, #1779, #12310 ) ) ;
#5419 = AXIS2_PLACEMENT_3D ( 'NONE', #10200, #1072, #5131 ) ;
#5420 = DIRECTION ( 'NONE',  ( 0.000000000000000000, 0.01970892327970883220, 0.9998057603070481525 ) ) ;
#5421 = LINE ( 'NONE', #9484, #5470 ) ;
#5422 = AXIS2_PLACEMENT_3D ( 'NONE', #538, #4585, #8729 ) ;
#5423 = CARTESIAN_POINT ( 'NONE',  ( 115.7315435905548071, 19.96883745941821786, 234.7354397751816180 ) ) ;
#5424 = EDGE_CURVE ( 'NONE', #9039, #10670, #3357, .T. ) ;
#5425 = CARTESIAN_POINT ( 'NONE',  ( -225.1241593668336236, -30.00000000000000000, 185.9653539489990521 ) ) ;
#5426 = DIRECTION ( 'NONE',  ( 0.08715574274765504337, 0.000000000000000000, 0.9961946980917459893 ) ) ;
#5427 = DIRECTION ( 'NONE',  ( 0.000000000000000000, -1.000000000000000000, 0.000000000000000000 ) ) ;
#5428 = DIRECTION ( 'NONE',  ( 0.000000000000000000, 0.9998057603070481525, -0.01970892327970899874 ) ) ;
#5429 = CIRCLE ( 'NONE', #8556, 240.3921568627449687 ) ;
#5430 = ORIENTED_EDGE ( 'NONE', *, *, #11663, .T. ) ;
#5431 = DIRECTION ( 'NONE',  ( 0.000000000000000000, 1.000000000000000000, 0.000000000000000000 ) ) ;
#5432 = EDGE_CURVE ( 'NONE', #2079, #1416, #11217, .T. ) ;
#5433 = ORIENTED_EDGE ( 'NONE', *, *, #4371, .F. ) ;
#5434 = DIRECTION ( 'NONE',  ( 0.000000000000000000, 1.000000000000000000, 0.000000000000000000 ) ) ;
#5435 = ORIENTED_EDGE ( 'NONE', *, *, #708, .T. ) ;
#5436 = ORIENTED_EDGE ( 'NONE', *, *, #3627, .T. ) ;
#5437 = PRESENTATION_LAYER_ASSIGNMENT (  '', '', ( #9477 ) ) ;
#5438 = PRODUCT_DEFINITION_SHAPE ( 'NONE', 'NONE',  #13064 ) ;
#5439 = CARTESIAN_POINT ( 'NONE',  ( 71.82423009839129691, 28.60000000000000142, 202.4354503650404808 ) ) ;
#5440 = DIRECTION ( 'NONE',  ( 0.000000000000000000, 0.000000000000000000, 1.000000000000000000 ) ) ;
#5441 = CARTESIAN_POINT ( 'NONE',  ( -238.7109915775760669, 0.006370638632528863136, -11.75000000064824768 ) ) ;
#5442 = CARTESIAN_POINT ( 'NONE',  ( -138.9238112054132444, -22.00000000000000000, 212.6409525001303678 ) ) ;
#5443 = ORIENTED_EDGE ( 'NONE', *, *, #4183, .F. ) ;
#5444 = CARTESIAN_POINT ( 'NONE',  ( 0.000000000000000000, 0.000000000000000000, 258.0000000000000000 ) ) ;
#5445 = CIRCLE ( 'NONE', #7999, 5.099999999999993427 ) ;
#5446 = VERTEX_POINT ( 'NONE', #10414 ) ;
#5447 = DIRECTION ( 'NONE',  ( 0.000000000000000000, 0.000000000000000000, 1.000000000000000000 ) ) ;
#5448 = CARTESIAN_POINT ( 'NONE',  ( 0.000000000000000000, 24.99999999999995737, 0.000000000000000000 ) ) ;
#5449 = CARTESIAN_POINT ( 'NONE',  ( 246.8597181602070521, 20.08915143297736705, -83.79436865282332292 ) ) ;
#5450 = CARTESIAN_POINT ( 'NONE',  ( -31.82909658242962792, -30.00000000000000000, 285.6728570749452274 ) ) ;
#5451 = CARTESIAN_POINT ( 'NONE',  ( -244.4430806157185430, 8.412306931070002491, -8.557769321120538564 ) ) ;
#5452 = CARTESIAN_POINT ( 'NONE',  ( -239.5718914762306611, 1.891487839302555374, 11.85001484810088535 ) ) ;
#5453 = CARTESIAN_POINT ( 'NONE',  ( -241.3664650619595022, -5.412961098251741987, -10.42892899848466115 ) ) ;
#5454 = ADVANCED_FACE ( 'NONE', ( #1289 ), #5063, .T. ) ;
#5455 = CARTESIAN_POINT ( 'NONE',  ( 0.000000000000000000, 9.997999799959989886, 0.000000000000000000 ) ) ;
#5456 =( NAMED_UNIT ( * ) PLANE_ANGLE_UNIT ( ) SI_UNIT ( $, .RADIAN. ) );
#5457 = CARTESIAN_POINT ( 'NONE',  ( -229.7326367665251894, 4.595192083928767879, -11.08697888960004896 ) ) ;
#5458 = ITEM_DEFINED_TRANSFORMATION ( 'NONE', 'NONE', #1501,  #805 ) ;
#5459 = B_SPLINE_CURVE_WITH_KNOTS ( 'NONE', 3,
 ( #6890, #6760, #12746, #9941, #5619, #12943, #7680, #1686, #760, #9809, #8819, #8880, #6823 ),
 .UNSPECIFIED., .F., .F.,
 ( 4, 2, 2, 1, 2, 2, 4 ),
 ( 0.000000000000000000, 0.2499999999999875655, 0.3749999999999813483, 0.4374999999999648614, 0.4687499999999565903, 0.4999999999999483191, 1.000000000000000000 ),
 .UNSPECIFIED. ) ;
#5460 = DIRECTION ( 'NONE',  ( 0.000000000000000000, 0.000000000000000000, 1.000000000000000000 ) ) ;
#5461 = ORIENTED_EDGE ( 'NONE', *, *, #4667, .T. ) ;
#5462 = CARTESIAN_POINT ( 'NONE',  ( -17.10461161519512174, 20.55460285096646089, 261.3381329044966606 ) ) ;
#5463 = DIRECTION ( 'NONE',  ( -0.000000000000000000, -1.000000000000000000, 0.000000000000000000 ) ) ;
#5464 = DIRECTION ( 'NONE',  ( 0.6368676505102696117, 0.000000000000000000, 0.7709731485165545184 ) ) ;
#5465 = CARTESIAN_POINT ( 'NONE',  ( 193.6077657551222444, -18.00000000000000000, 234.3758371490322361 ) ) ;
#5466 = CARTESIAN_POINT ( 'NONE',  ( -190.2689011420773966, 20.08915143297736705, 178.2104428091925001 ) ) ;
#5467 = EDGE_CURVE ( 'NONE', #6909, #6421, #6158, .T. ) ;
#5468 = EDGE_CURVE ( 'NONE', #10757, #8455, #6784, .T. ) ;
#5469 = FACE_OUTER_BOUND ( 'NONE', #2902, .T. ) ;
#5470 = VECTOR ( 'NONE', #5545, 1000.000000000000114 ) ;
#5471 = DIRECTION ( 'NONE',  ( -0.7210484489137172215, 0.5538822189107471816, -0.4162975160791012597 ) ) ;
#5472 = CARTESIAN_POINT ( 'NONE',  ( -246.2764285590020279, -9.322503223484712720, 7.152604638120487301 ) ) ;
#5473 = CARTESIAN_POINT ( 'NONE',  ( 197.8197553893915028, 19.00000000000000000, -64.27553482998990830 ) ) ;
#5474 = CARTESIAN_POINT ( 'NONE',  ( 6.345753394971347358E-13, 20.08915143297736350, -260.5542428351130866 ) ) ;
#5475 = VERTEX_POINT ( 'NONE', #2475 ) ;
#5476 = ORIENTED_EDGE ( 'NONE', *, *, #12187, .T. ) ;
#5477 = ADVANCED_FACE ( 'NONE', ( #11556 ), #1029, .T. ) ;
#5478 = CARTESIAN_POINT ( 'NONE',  ( -228.6269314446401211, -29.00000000000000000, 181.7250016321579835 ) ) ;
#5479 = DIRECTION ( 'NONE',  ( 0.000000000000000000, -1.000000000000000000, 0.000000000000000000 ) ) ;
#5480 = CARTESIAN_POINT ( 'NONE',  ( -84.20717312421410838, 20.55460285060721048, -247.9906035374705766 ) ) ;
#5481 = AXIS2_PLACEMENT_3D ( 'NONE', #1662, #12925, #11808 ) ;
#5482 = DIRECTION ( 'NONE',  ( 0.000000000000000000, 0.000000000000000000, 1.000000000000000000 ) ) ;
#5483 =( REPRESENTATION_RELATIONSHIP ('NONE','NONE', #12019, #182 ) REPRESENTATION_RELATIONSHIP_WITH_TRANSFORMATION ( #7843 )SHAPE_REPRESENTATION_RELATIONSHIP( ) );
#5484 = DIRECTION ( 'NONE',  ( -0.3420201433256726542, 0.000000000000000000, 0.9396926207859069846 ) ) ;
#5485 = CARTESIAN_POINT ( 'NONE',  ( -122.2593324768359935, 19.00000000000000000, -168.2755348299880040 ) ) ;
#5486 = CARTESIAN_POINT ( 'NONE',  ( -34.05310945292020364, 20.79694577634647246, 258.6823826759385270 ) ) ;
#5487 = ORIENTED_EDGE ( 'NONE', *, *, #2369, .F. ) ;
#5488 = CARTESIAN_POINT ( 'NONE',  ( 172.0303573358525284, 20.79694577634646535, -196.1676464792605259 ) ) ;
#5489 = ORIENTED_EDGE ( 'NONE', *, *, #6073, .F. ) ;
#5490 = CARTESIAN_POINT ( 'NONE',  ( -210.0000000000000000, 30.00000000000000000, 0.000000000000000000 ) ) ;
#5491 = ORIENTED_EDGE ( 'NONE', *, *, #9803, .T. ) ;
#5492 = ORIENTED_EDGE ( 'NONE', *, *, #10724, .T. ) ;
#5493 = EDGE_CURVE ( 'NONE', #11582, #158, #1417, .T. ) ;
#5494 = EDGE_CURVE ( 'NONE', #11715, #3954, #1546, .T. ) ;
#5495 = DIRECTION ( 'NONE',  ( 0.6368676505102716101, 0.000000000000000000, 0.7709731485165527420 ) ) ;
#5496 = DIRECTION ( 'NONE',  ( 0.000000000000000000, -1.000000000000000000, 0.000000000000000000 ) ) ;
#5497 = B_SPLINE_CURVE_WITH_KNOTS ( 'NONE', 3,
 ( #8846, #1783, #7707, #11721, #4629, #5851, #3711, #10841, #8977, #12774, #6918, #6846, #6783 ),
 .UNSPECIFIED., .F., .F.,
 ( 4, 2, 2, 1, 2, 2, 4 ),
 ( 0.000000000000000000, 0.2500000000000000555, 0.5000000000000001110, 0.6250000000000001110, 0.6875000000000000000, 0.7499999999999998890, 1.000000000000000000 ),
 .UNSPECIFIED. ) ;
#5498 = LINE ( 'NONE', #12635, #11553 ) ;
#5499 = LINE ( 'NONE', #3353, #6700 ) ;
#5500 = DIRECTION ( 'NONE',  ( 0.000000000000000000, 0.000000000000000000, 1.000000000000000000 ) ) ;
#5501 = CIRCLE ( 'NONE', #7204, 5.500000000000005329 ) ;
#5502 = VECTOR ( 'NONE', #1139, 1000.000000000000227 ) ;
#5503 = AXIS2_PLACEMENT_3D ( 'NONE', #5617, #7555, #493 ) ;
#5504 = CONTEXT_DEPENDENT_SHAPE_REPRESENTATION ( #11190, #11050 ) ;
#5505 = ORIENTED_EDGE ( 'NONE', *, *, #1165, .T. ) ;
#5506 = VECTOR ( 'NONE', #483, 1000.000000000000000 ) ;
#5507 = CARTESIAN_POINT ( 'NONE',  ( -122.2593324768359935, 30.00000000000000000, -161.7755348299880040 ) ) ;
#5508 = VERTEX_POINT ( 'NONE', #5478 ) ;
#5509 = CARTESIAN_POINT ( 'NONE',  ( 71.82423009839129691, 28.60000000000000142, 197.3354503650404865 ) ) ;
#5510 = DIRECTION ( 'NONE',  ( 0.000000000000000000, 0.9998057603070480415, -0.01970892327970899874 ) ) ;
#5511 = B_SPLINE_CURVE_WITH_KNOTS ( 'NONE', 3,
 ( #9751, #1701, #3757, #7822, #638, #11896, #772, #2759, #3146, #2029, #5222, #3959, #1026, #11294, #12162, #7692, #899, #12293, #4023, #7296, #2087, #8101, #2951, #9231, #3015, #9294, #6100, #11094, #5085, #8031, #9160, #36, #3216, #12363, #2224, #7098, #4157, #12093, #10151, #8238, #1962, #1094, #102, #4218, #11364, #8303, #9096, #6037, #11160, #7233, #4090, #6303, #166, #8170, #10092, #3086, #4957, #12231, #7164, #9034, #7033, #2158, #11223, #6166, #966, #5023, #10220, #6236, #5151, #10288, #1163, #2547, #1424, #10617, #2420, #12488, #12430, #4287, #362, #9362, #1226 ),
 .UNSPECIFIED., .F., .F.,
 ( 4, 1, 1, 1, 2, 2, 2, 1, 1, 1, 2, 2, 2, 2, 1, 1, 1, 1, 2, 2, 2, 2, 1, 1, 1, 2, 2, 2, 1, 1, 1, 2, 2, 2, 2, 1, 1, 1, 2, 2, 2, 1, 1, 1, 2, 2, 2, 1, 1, 1, 2, 2, 4 ),
 ( 0.000000000000000000, 0.03124999999994631378, 0.04687499999991946720, 0.05468749999990599880, 0.05859374999989923338, 0.06249999999989246796, 0.09374999999987096433, 0.1093749999998601952, 0.1171874999998548522, 0.1210937499998521738, 0.1230468749998536865, 0.1249999999998551992, 0.1875000000000294764, 0.2187500000001137146, 0.2343750000001531830, 0.2421875000001753597, 0.2460937500001839640, 0.2480468750001859068, 0.2490234375001867950, 0.2500000000001876832, 0.3125000000001743050, 0.3437500000001676437, 0.3593750000001619815, 0.3671875000001592615, 0.3710937500001600386, 0.3730468750001624811, 0.3750000000001648681, 0.4375000000001639244, 0.4687500000001658118, 0.4843750000001668665, 0.4921875000001651457, 0.4960937500001642575, 0.5000000000001634248, 0.5625000000001737499, 0.5937500000001809664, 0.6093750000001847411, 0.6171875000001865175, 0.6210937500001851852, 0.6230468750001870726, 0.6250000000001889600, 0.6875000000001727507, 0.7187500000001628697, 0.7343750000001598721, 0.7421875000001600942, 0.7460937500001600942, 0.7500000000001599831, 0.8125000000001328937, 0.8437500000001192380, 0.8593750000001121325, 0.8671875000001085798, 0.8710937500001052491, 0.8750000000001018075, 1.000000000000000000 ),
 .UNSPECIFIED. ) ;
#5512 = ADVANCED_FACE ( 'NONE', ( #356 ), #12546, .F. ) ;
#5513 = VECTOR ( 'NONE', #8133, 1000.000000000000000 ) ;
#5514 = CYLINDRICAL_SURFACE ( 'NONE', #12560, 5.100000000000003197 ) ;
#5515 = LINE ( 'NONE', #2693, #7899 ) ;
#5516 = FACE_OUTER_BOUND ( 'NONE', #5889, .T. ) ;
#5517 = CARTESIAN_POINT ( 'NONE',  ( 220.3999999999999773, -0.9998057603070324983, 0.01970892327970881139 ) ) ;
#5518 = VECTOR ( 'NONE', #11018, 1000.000000000000000 ) ;
#5519 = VECTOR ( 'NONE', #7465, 1000.000000000000227 ) ;
#5520 = CARTESIAN_POINT ( 'NONE',  ( -239.9450917581424960, 2.156506209390990136, -11.80463811257499884 ) ) ;
#5521 = PRODUCT_CONTEXT ( 'NONE', #12327, 'mechanical' ) ;
#5522 = CARTESIAN_POINT ( 'NONE',  ( -229.8898327533349573, 9.665891927765104086, 7.128580859766620925 ) ) ;
#5523 = CONTEXT_DEPENDENT_SHAPE_REPRESENTATION ( #3133, #6539 ) ;
#5524 = CONICAL_SURFACE ( 'NONE', #5948, 5.500000000000015099, 0.7853981633974461696 ) ;
#5525 = DIRECTION ( 'NONE',  ( 0.000000000000000000, 0.000000000000000000, -1.000000000000000000 ) ) ;
#5526 = VERTEX_POINT ( 'NONE', #5544 ) ;
#5527 = CARTESIAN_POINT ( 'NONE',  ( 261.1558126970361400, 19.96883746059272724, -17.09264059807959057 ) ) ;
#5528 = CARTESIAN_POINT ( 'NONE',  ( 0.000000000000000000, 0.000000000000000000, 0.000000000000000000 ) ) ;
#5529 = DIRECTION ( 'NONE',  ( 0.6368676505102707219, 0.000000000000000000, 0.7709731485165535192 ) ) ;
#5530 = LINE ( 'NONE', #9471, #10429 ) ;
#5531 = CIRCLE ( 'NONE', #11061, 239.8169934640564804 ) ;
#5532 = FACE_BOUND ( 'NONE', #12490, .T. ) ;
#5533 = CARTESIAN_POINT ( 'NONE',  ( 227.3999999999999773, -0.1281080013181084831, -6.498737441995811714 ) ) ;
#5534 = CARTESIAN_POINT ( 'NONE',  ( -37.93010648591162237, -138.4705547276867321, -17.68709912901536896 ) ) ;
#5535 = CARTESIAN_POINT ( 'NONE',  ( -229.7148377869573608, -2.666494325112176433, -11.44984222230669069 ) ) ;
#5536 = CONTEXT_DEPENDENT_SHAPE_REPRESENTATION ( #3446, #4105 ) ;
#5537 = CARTESIAN_POINT ( 'NONE',  ( 0.000000000000000000, 18.00000000000000000, 0.000000000000000000 ) ) ;
#5538 = CARTESIAN_POINT ( 'NONE',  ( -229.7320401093896578, -4.610569389177691768, 11.10393803714480754 ) ) ;
#5539 = ORIENTED_EDGE ( 'NONE', *, *, #10116, .T. ) ;
#5540 = ADVANCED_FACE ( 'NONE', ( #8552 ), #7485, .F. ) ;
#5541 = ORIENTED_EDGE ( 'NONE', *, *, #9993, .T. ) ;
#5542 = EDGE_CURVE ( 'NONE', #6354, #6448, #3998, .T. ) ;
#5543 = AXIS2_PLACEMENT_3D ( 'NONE', #9328, #2192, #198 ) ;
#5544 = CARTESIAN_POINT ( 'NONE',  ( 228.6269314446401211, -19.00000000000000000, -181.7250016321579835 ) ) ;
#5545 = DIRECTION ( 'NONE',  ( 8.659560562354913137E-17, -0.7071067811865489050, 0.7071067811865460184 ) ) ;
#5546 = CIRCLE ( 'NONE', #3840, 249.0000000000000284 ) ;
#5547 = CARTESIAN_POINT ( 'NONE',  ( 34.20858920406338655, 20.55460285047751157, -259.6535381481361355 ) ) ;
#5548 = LINE ( 'NONE', #9806, #11571 ) ;
#5549 = CARTESIAN_POINT ( 'NONE',  ( 0.000000000000000000, 0.000000000000000000, 0.000000000000000000 ) ) ;
#5550 = DIRECTION ( 'NONE',  ( 0.000000000000000000, -1.000000000000000000, 0.000000000000000000 ) ) ;
#5551 = CARTESIAN_POINT ( 'NONE',  ( -258.6823826759384701, 20.79694577634646535, -34.05310945291999047 ) ) ;
#5552 = PRODUCT_DEFINITION_FORMATION_WITH_SPECIFIED_SOURCE ( 'ANY', '', #3805, .NOT_KNOWN. ) ;
#5553 = EDGE_LOOP ( 'NONE', ( #3820, #11857 ) ) ;
#5554 = FACE_OUTER_BOUND ( 'NONE', #2599, .T. ) ;
#5555 = ORIENTED_EDGE ( 'NONE', *, *, #3335, .F. ) ;
#5556 = DIRECTION ( 'NONE',  ( 0.000000000000000000, 0.000000000000000000, 1.000000000000000000 ) ) ;
#5557 = ORIENTED_EDGE ( 'NONE', *, *, #7831, .F. ) ;
#5558 = VERTEX_POINT ( 'NONE', #488 ) ;
#5559 = CARTESIAN_POINT ( 'NONE',  ( 0.000000000000000000, 0.000000000000000000, 0.000000000000000000 ) ) ;
#5560 = VECTOR ( 'NONE', #12171, 1000.000000000000000 ) ;
#5561 = CARTESIAN_POINT ( 'NONE',  ( -207.7919029844864269, 20.55460285060714654, 159.4136521835260112 ) ) ;
#5562 = DIRECTION ( 'NONE',  ( -1.000000000000000000, 0.000000000000000000, 0.000000000000000000 ) ) ;
#5563 = CARTESIAN_POINT ( 'NONE',  ( 239.0530249120305371, 0.6193663070761113998, -3.444815813553090411 ) ) ;
#5564 = CARTESIAN_POINT ( 'NONE',  ( -238.7118983370134799, 0.07231316710876492526, -11.74979690964867807 ) ) ;
#5565 =( NAMED_UNIT ( * ) SI_UNIT ( $, .STERADIAN. ) SOLID_ANGLE_UNIT ( ) );
#5566 = CARTESIAN_POINT ( 'NONE',  ( 0.000000000000000000, 30.00000000000000000, 0.000000000000000000 ) ) ;
#5567 = ADVANCED_FACE ( 'NONE', ( #6553 ), #8282, .F. ) ;
#5568 = EDGE_CURVE ( 'NONE', #1635, #6293, #2367, .T. ) ;
#5569 = ITEM_DEFINED_TRANSFORMATION ( 'NONE', 'NONE', #5282,  #805 ) ;
#5570 = VERTEX_POINT ( 'NONE', #12733 ) ;
#5571 = DIRECTION ( 'NONE',  ( -1.000000000000000000, 0.000000000000000000, 0.000000000000000000 ) ) ;
#5572 = ORIENTED_EDGE ( 'NONE', *, *, #2705, .F. ) ;
#5573 = CARTESIAN_POINT ( 'NONE',  ( -243.1551830321994316, 7.446108171819295407, -9.089443071765307636 ) ) ;
#5574 = CARTESIAN_POINT ( 'NONE',  ( 0.000000000000000000, -9.830508068699650437, 0.000000000000000000 ) ) ;
#5575 = VECTOR ( 'NONE', #11377, 1000.000000000000114 ) ;
#5576 = DIRECTION ( 'NONE',  ( -0.000000000000000000, -1.000000000000000000, 0.000000000000000000 ) ) ;
#5577 = DIRECTION ( 'NONE',  ( 0.6368676505102707219, 0.000000000000000000, 0.7709731485165535192 ) ) ;
#5578 = DIRECTION ( 'NONE',  ( -0.000000000000000000, -1.000000000000000000, 0.000000000000000000 ) ) ;
#5579 = AXIS2_PLACEMENT_3D ( 'NONE', #11619, #4465, #6488 ) ;
#5580 = CARTESIAN_POINT ( 'NONE',  ( -240.7431671956743173, -4.340241521192577778, -10.91924886806390838 ) ) ;
#5581 = CARTESIAN_POINT ( 'NONE',  ( -249.5626403297915772, -9.995018771280594905, 6.640755139178303956 ) ) ;
#5582 = CONICAL_SURFACE ( 'NONE', #8997, 261.0000000000000000, 1.373400766945014784 ) ;
#5583 = EDGE_CURVE ( 'NONE', #9146, #4062, #4469, .T. ) ;
#5584 = CARTESIAN_POINT ( 'NONE',  ( 220.3999999999999773, 0.000000000000000000, 0.000000000000000000 ) ) ;
#5585 = DIRECTION ( 'NONE',  ( 0.9396926207859126468, 0.000000000000000000, -0.3420201433256568890 ) ) ;
#5586 = AXIS2_PLACEMENT_3D ( 'NONE', #11575, #2432, #6514 ) ;
#5587 = CARTESIAN_POINT ( 'NONE',  ( -229.9651316831089787, 11.31282158159266693, 4.019724534361353463 ) ) ;
#5588 = EDGE_CURVE ( 'NONE', #5106, #2886, #191, .T. ) ;
#5589 = ORIENTED_EDGE ( 'NONE', *, *, #12425, .T. ) ;
#5590 = LINE ( 'NONE', #1400, #10834 ) ;
#5591 = ORIENTED_EDGE ( 'NONE', *, *, #10968, .F. ) ;
#5592 = TOROIDAL_SURFACE ( 'NONE', #8791, 241.5000000000000000, 2.500000000000000000 ) ;
#5593 =( REPRESENTATION_RELATIONSHIP ('NONE','NONE', #12019, #5191 ) REPRESENTATION_RELATIONSHIP_WITH_TRANSFORMATION ( #4725 )SHAPE_REPRESENTATION_RELATIONSHIP( ) );
#5594 = CARTESIAN_POINT ( 'NONE',  ( 247.8175805191053769, 19.96883746103348045, -84.14846197955421303 ) ) ;
#5595 = FACE_OUTER_BOUND ( 'NONE', #12154, .T. ) ;
#5596 = FACE_OUTER_BOUND ( 'NONE', #7297, .T. ) ;
#5597 = VECTOR ( 'NONE', #1772, 1000.000000000000000 ) ;
#5598 = CARTESIAN_POINT ( 'NONE',  ( -250.0000000000000000, 0.000000000000000000, -12.00000000000000000 ) ) ;
#5599 = CARTESIAN_POINT ( 'NONE',  ( -240.0092717900960793, 2.435426587042586188, 11.75368411291894688 ) ) ;
#5600 = CARTESIAN_POINT ( 'NONE',  ( 0.000000000000000000, 0.000000000000000000, 0.000000000000000000 ) ) ;
#5601 = CARTESIAN_POINT ( 'NONE',  ( -20.92562098022552064, -138.4705547276867321, 36.24423871767976379 ) ) ;
#5602 = CIRCLE ( 'NONE', #10281, 239.0000000000000000 ) ;
#5603 = VECTOR ( 'NONE', #10962, 1000.000000000000000 ) ;
#5604 = CARTESIAN_POINT ( 'NONE',  ( -229.8108972436801594, -7.155453164010755707, -9.328021014420249557 ) ) ;
#5605 = CONICAL_SURFACE ( 'NONE', #9014, 5.100000000000003197, 0.7853981633974503884 ) ;
#5606 = ITEM_DEFINED_TRANSFORMATION ( 'NONE', 'NONE', #11252,  #805 ) ;
#5607 = VECTOR ( 'NONE', #8625, 1000.000000000000000 ) ;
#5608 = CARTESIAN_POINT ( 'NONE',  ( -241.0259582380425911, -4.889855348568320714, -10.95996151980668643 ) ) ;
#5609 = CARTESIAN_POINT ( 'NONE',  ( -229.8758510084904572, -9.325226166226105562, 7.561748853445185325 ) ) ;
#5610 = ORIENTED_EDGE ( 'NONE', *, *, #8812, .T. ) ;
#5611 = VERTEX_POINT ( 'NONE', #3670 ) ;
#5612 = CARTESIAN_POINT ( 'NONE',  ( 122.2593324768334071, 29.00000000000000000, -168.2755348299895104 ) ) ;
#5613 = DIRECTION ( 'NONE',  ( 1.000000000000000000, 0.000000000000000000, 0.000000000000000000 ) ) ;
#5614 = AXIS2_PLACEMENT_3D ( 'NONE', #1209, #1142, #345 ) ;
#5615 = CARTESIAN_POINT ( 'NONE',  ( -234.3927740973375080, 20.79694577663154575, -115.5625104413860100 ) ) ;
#5616 = CARTESIAN_POINT ( 'NONE',  ( -239.5361044668159991, -1.848645179572815156, -11.60366368868215758 ) ) ;
#5617 = CARTESIAN_POINT ( 'NONE',  ( 0.000000000000000000, 0.000000000000000000, 0.000000000000000000 ) ) ;
#5618 = CARTESIAN_POINT ( 'NONE',  ( 0.000000000000000000, -1.848645179579245124, 0.000000000000000000 ) ) ;
#5619 = CARTESIAN_POINT ( 'NONE',  ( 240.0731061099968429, 2.151402440697789853, -2.761193928003757847 ) ) ;
#5620 = ADVANCED_FACE ( 'NONE', ( #10606 ), #1457, .F. ) ;
#5621 = ORIENTED_EDGE ( 'NONE', *, *, #4895, .T. ) ;
#5622 = CARTESIAN_POINT ( 'NONE',  ( 115.4021059068220438, 20.79694577634646890, -234.0054343868617366 ) ) ;
#5623 = VECTOR ( 'NONE', #6710, 1000.000000000000114 ) ;
#5624 = ORIENTED_EDGE ( 'NONE', *, *, #12015, .F. ) ;
#5625 = CARTESIAN_POINT ( 'NONE',  ( -27.68945685411286561, -18.00000000000000000, 290.6841825403027997 ) ) ;
#5626 = ORIENTED_EDGE ( 'NONE', *, *, #5009, .T. ) ;
#5627 = ORIENTED_EDGE ( 'NONE', *, *, #3655, .F. ) ;
#5628 =( BOUNDED_CURVE ( )  B_SPLINE_CURVE ( 3, ( #2464, #12664, #9657, #10534 ),
 .UNSPECIFIED., .F., .F. ) 
 B_SPLINE_CURVE_WITH_KNOTS ( ( 4, 4 ),
 ( 0.000000000000000000, 1.000000000000000000 ),
 .UNSPECIFIED. ) 
 CURVE ( )  GEOMETRIC_REPRESENTATION_ITEM ( )  RATIONAL_B_SPLINE_CURVE ( ( 1.000000000000000000, 0.4027746460044325238, 0.4027746460044325238, 1.000000000000000000 ) ) 
 REPRESENTATION_ITEM ( '' )  );
#5629 = VERTEX_POINT ( 'NONE', #6619 ) ;
#5630 = DIRECTION ( 'NONE',  ( 0.000000000000000000, 0.000000000000000000, 1.000000000000000000 ) ) ;
#5631 = DIRECTION ( 'NONE',  ( -0.4503334343941441942, 0.7071067811865670016, -0.5451603414287832239 ) ) ;
#5632 = LINE ( 'NONE', #11963, #3237 ) ;
#5633 = AXIS2_PLACEMENT_3D ( 'NONE', #6071, #2060, #7069 ) ;
#5634 = CARTESIAN_POINT ( 'NONE',  ( 0.000000000000000000, 0.000000000000000000, 0.000000000000000000 ) ) ;
#5635 =( NAMED_UNIT ( * ) SI_UNIT ( $, .STERADIAN. ) SOLID_ANGLE_UNIT ( ) );
#5636 = PRESENTATION_STYLE_ASSIGNMENT (( #444 ) ) ;
#5637 = EDGE_CURVE ( 'NONE', #3848, #5028, #8055, .T. ) ;
#5638 = ITEM_DEFINED_TRANSFORMATION ( 'NONE', 'NONE', #3152,  #805 ) ;
#5639 = ORIENTED_EDGE ( 'NONE', *, *, #4433, .T. ) ;
#5640 = CARTESIAN_POINT ( 'NONE',  ( -238.9974237869947444, -1.159187598540258213, 11.69290073402236985 ) ) ;
#5641 = ORIENTED_EDGE ( 'NONE', *, *, #306, .T. ) ;
#5642 = LINE ( 'NONE', #1445, #4789 ) ;
#5643 = VERTEX_POINT ( 'NONE', #553 ) ;
#5644 = EDGE_CURVE ( 'NONE', #6599, #6354, #8675, .T. ) ;
#5645 = FACE_OUTER_BOUND ( 'NONE', #7443, .T. ) ;
#5646 = DIRECTION ( 'NONE',  ( 0.000000000000000000, 0.000000000000000000, 1.000000000000000000 ) ) ;
#5647 = DIRECTION ( 'NONE',  ( -0.000000000000000000, -1.000000000000000000, 0.000000000000000000 ) ) ;
#5648 = CARTESIAN_POINT ( 'NONE',  ( -229.9254091646820370, 10.19501318499466613, 5.891900222926529374 ) ) ;
#5649 = DIRECTION ( 'NONE',  ( 0.6368676505102716101, 0.000000000000000000, 0.7709731485165527420 ) ) ;
#5650 = AXIS2_PLACEMENT_3D ( 'NONE', #3575, #4634, #7647 ) ;
#5651 = DIRECTION ( 'NONE',  ( 0.000000000000000000, 0.9998057603070480415, -0.01970892327970899874 ) ) ;
#5652 = APPLICATION_PROTOCOL_DEFINITION ( 'draft international standard', 'automotive_design', 1998, #3002 ) ;
#5653 = AXIS2_PLACEMENT_3D ( 'NONE', #2362, #3283, #12495 ) ;
#5654 = DIRECTION ( 'NONE',  ( 0.000000000000000000, -1.000000000000000000, 0.000000000000000000 ) ) ;
#5655 = VERTEX_POINT ( 'NONE', #7742 ) ;
#5656 = ORIENTED_EDGE ( 'NONE', *, *, #9595, .F. ) ;
#5657 = CARTESIAN_POINT ( 'NONE',  ( -249.7994671773518292, -11.75014634419642512, 0.3782188002307603214 ) ) ;
#5658 = ORIENTED_EDGE ( 'NONE', *, *, #2487, .T. ) ;
#5659 = ADVANCED_FACE ( 'NONE', ( #10743 ), #7415, .F. ) ;
#5660 = CARTESIAN_POINT ( 'NONE',  ( 67.71318189755788808, 19.96883746081500988, -252.8031682274115894 ) ) ;
#5661 = EDGE_CURVE ( 'NONE', #10688, #10559, #2091, .T. ) ;
#5662 = DIRECTION ( 'NONE',  ( -0.000000000000000000, -1.000000000000000000, 0.000000000000000000 ) ) ;
#5663 = DIRECTION ( 'NONE',  ( 1.000000000000000000, 0.000000000000000000, -0.000000000000000000 ) ) ;
#5664 = CARTESIAN_POINT ( 'NONE',  ( 222.0845275804282153, -1.749660080537334128, 0.03449061573949095683 ) ) ;
#5665 = CARTESIAN_POINT ( 'NONE',  ( -241.9271341497538970, 6.190796898938002002, 10.28045873024532320 ) ) ;
#5666 = EDGE_CURVE ( 'NONE', #9649, #779, #4861, .T. ) ;
#5667 = FACE_OUTER_BOUND ( 'NONE', #6276, .T. ) ;
#5668 = DIRECTION ( 'NONE',  ( -0.1445786100688048470, 0.5538822189107472926, -0.8199460427888410896 ) ) ;
#5669 = CARTESIAN_POINT ( 'NONE',  ( 229.9973455135990719, 3.322144853712378332, 1.125217561599514582 ) ) ;
#5670 = CARTESIAN_POINT ( 'NONE',  ( -249.6369960391239431, 11.07262528784599986, -3.948341302959084143 ) ) ;
#5671 = CARTESIAN_POINT ( 'NONE',  ( 225.1241593668336236, -30.00000000000000000, -185.9653539489990521 ) ) ;
#5672 = CARTESIAN_POINT ( 'NONE',  ( 27.68945685411497593, -19.00000000000000000, -290.6841825403026291 ) ) ;
#5673 = ORIENTED_EDGE ( 'NONE', *, *, #8441, .T. ) ;
#5674 = ORIENTED_EDGE ( 'NONE', *, *, #1828, .F. ) ;
#5675 =( REPRESENTATION_RELATIONSHIP ('NONE','NONE', #12019, #182 ) REPRESENTATION_RELATIONSHIP_WITH_TRANSFORMATION ( #4205 )SHAPE_REPRESENTATION_RELATIONSHIP( ) );
#5676 = DIRECTION ( 'NONE',  ( -0.000000000000000000, -1.000000000000000000, 0.000000000000000000 ) ) ;
#5677 = EDGE_CURVE ( 'NONE', #11199, #9111, #6357, .T. ) ;
#5678 = CARTESIAN_POINT ( 'NONE',  ( -122.2593324768359935, 30.00000000000000000, -173.7755348299880040 ) ) ;
#5679 = APPLICATION_CONTEXT ( 'automotive_design' ) ;
#5680 = CARTESIAN_POINT ( 'NONE',  ( -234.3927740981719978, 20.79694577626919028, 115.5625104415733944 ) ) ;
#5681 = DIRECTION ( 'NONE',  ( -0.000000000000000000, -1.000000000000000000, 0.000000000000000000 ) ) ;
#5682 = PRODUCT_DEFINITION_SHAPE ( 'NONE', 'NONE',  #13167 ) ;
#5683 = DIRECTION ( 'NONE',  ( -0.2588190451025247363, 0.000000000000000000, 0.9659258262890674240 ) ) ;
#5684 = CARTESIAN_POINT ( 'NONE',  ( 31.82909658243172757, -18.00000000000000000, -285.6728570749450569 ) ) ;
#5685 = DIRECTION ( 'NONE',  ( 0.000000000000000000, 0.000000000000000000, 1.000000000000000000 ) ) ;
#5686 = ORIENTED_EDGE ( 'NONE', *, *, #11342, .T. ) ;
#5687 = CARTESIAN_POINT ( 'NONE',  ( 27.68945685411497593, -29.00000000000000000, -290.6841825403026291 ) ) ;
#5688 = ORIENTED_EDGE ( 'NONE', *, *, #12273, .F. ) ;
#5689 = ORIENTED_EDGE ( 'NONE', *, *, #5737, .T. ) ;
#5690 = CARTESIAN_POINT ( 'NONE',  ( 211.9058003148608123, 20.08915143297736350, 151.8458048843642700 ) ) ;
#5691 = VERTEX_POINT ( 'NONE', #9073 ) ;
#5692 = PRODUCT_DEFINITION_SHAPE ( 'NONE', 'NONE',  #13146 ) ;
#5693 = LINE ( 'NONE', #7760, #7944 ) ;
#5694 = VECTOR ( 'NONE', #12843, 1000.000000000000000 ) ;
#5695 = DIRECTION ( 'NONE',  ( 0.000000000000000000, 0.000000000000000000, -1.000000000000000000 ) ) ;
#5696 = FACE_OUTER_BOUND ( 'NONE', #26, .T. ) ;
#5697 = CYLINDRICAL_SURFACE ( 'NONE', #4557, 5.499999999999998224 ) ;
#5698 = SHAPE_REPRESENTATION_RELATIONSHIP ( 'NONE' , 'NONE' ,  #11156, #12065 ) ;
#5699 = DIRECTION ( 'NONE',  ( 0.000000000000000000, 0.000000000000000000, 1.000000000000000000 ) ) ;
#5700 = ORIENTED_EDGE ( 'NONE', *, *, #11027, .T. ) ;
#5701 = FACE_OUTER_BOUND ( 'NONE', #5380, .T. ) ;
#5702 = ORIENTED_EDGE ( 'NONE', *, *, #9422, .F. ) ;
#5703 = CARTESIAN_POINT ( 'NONE',  ( -241.2893272559224158, 5.295647552975790262, -10.48903809278043120 ) ) ;
#5704 = ORIENTED_EDGE ( 'NONE', *, *, #12058, .T. ) ;
#5705 = EDGE_CURVE ( 'NONE', #7072, #497, #3151, .T. ) ;
#5706 = ADVANCED_FACE ( 'NONE', ( #12937 ), #12320, .T. ) ;
#5707 = DIRECTION ( 'NONE',  ( 0.000000000000000000, 0.000000000000000000, -1.000000000000000000 ) ) ;
#5708 = DIRECTION ( 'NONE',  ( 0.6368676505102689456, 0.000000000000000000, 0.7709731485165549625 ) ) ;
#5709 = CARTESIAN_POINT ( 'NONE',  ( 194.2446334056325554, -19.00000000000000000, 235.1468102975488250 ) ) ;
#5710 = DIRECTION ( 'NONE',  ( -0.000000000000000000, -1.000000000000000000, 0.000000000000000000 ) ) ;
#5711 = AXIS2_PLACEMENT_3D ( 'NONE', #8749, #10948, #9940 ) ;
#5712 = CARTESIAN_POINT ( 'NONE',  ( -242.3537289171788132, -6.680330752951019413, 9.968624626860709270 ) ) ;
#5713 = CARTESIAN_POINT ( 'NONE',  ( 235.0999999999999943, -2.749465840844381948, 0.05419953901920007699 ) ) ;
#5714 = CONTEXT_DEPENDENT_SHAPE_REPRESENTATION ( #5253, #5840 ) ;
#5715 = EDGE_LOOP ( 'NONE', ( #11385, #12282, #2374, #3649 ) ) ;
#5716 = DIRECTION ( 'NONE',  ( 0.000000000000000000, 1.000000000000000000, 0.000000000000000000 ) ) ;
#5717 = ORIENTED_EDGE ( 'NONE', *, *, #12845, .F. ) ;
#5718 = CIRCLE ( 'NONE', #1520, 6.500000000000005329 ) ;
#5719 = PRODUCT_DEFINITION_SHAPE ( 'NONE', 'NONE',  #13056 ) ;
#5720 = ORIENTED_EDGE ( 'NONE', *, *, #8795, .T. ) ;
#5721 = CARTESIAN_POINT ( 'NONE',  ( -248.2181897918291895, -9.855491095783875721, -6.397958699636017599 ) ) ;
#5722 = AXIS2_PLACEMENT_3D ( 'NONE', #957, #2872, #9024 ) ;
#5723 = EDGE_LOOP ( 'NONE', ( #6855, #11215, #9299, #7037 ) ) ;
#5724 = CONICAL_SURFACE ( 'NONE', #10404, 5.099999999999993427, 0.7853981633974461696 ) ;
#5725 = CARTESIAN_POINT ( 'NONE',  ( 196.8887528220037950, 20.55460285134802589, -172.6991790960863966 ) ) ;
#5726 = CARTESIAN_POINT ( 'NONE',  ( 235.4000000000000057, 0.000000000000000000, 0.000000000000000000 ) ) ;
#5727 = DIRECTION ( 'NONE',  ( 0.000000000000000000, -1.000000000000000000, 0.000000000000000000 ) ) ;
#5728 = AXIS2_PLACEMENT_3D ( 'NONE', #12337, #1267, #9070 ) ;
#5729 = CARTESIAN_POINT ( 'NONE',  ( 0.000000000000000000, -22.00000000000000000, 0.000000000000000000 ) ) ;
#5730 = CARTESIAN_POINT ( 'NONE',  ( -240.0865915474595624, 2.714760371449491227, 11.69235895546072790 ) ) ;
#5731 = AXIS2_PLACEMENT_3D ( 'NONE', #2758, #11846, #9699 ) ;
#5732 = FACE_OUTER_BOUND ( 'NONE', #10428, .T. ) ;
#5733 = CARTESIAN_POINT ( 'NONE',  ( -20.92562098022526840, -138.4705547276867321, -36.24423871767990590 ) ) ;
#5734 = EDGE_CURVE ( 'NONE', #6766, #2870, #4870, .T. ) ;
#5735 = CARTESIAN_POINT ( 'NONE',  ( 229.9748299376111333, 0.9217590672928105411, 3.407079461714101143 ) ) ;
#5736 = ITEM_DEFINED_TRANSFORMATION ( 'NONE', 'NONE', #1932,  #805 ) ;
#5737 = EDGE_CURVE ( 'NONE', #6137, #8105, #8074, .T. ) ;
#5738 = CARTESIAN_POINT ( 'NONE',  ( -248.5980333530941380, 9.980365686252888224, -6.207212897962511633 ) ) ;
#5739 = CARTESIAN_POINT ( 'NONE',  ( 0.000000000000000000, 30.00000000000000000, -208.0000000000000000 ) ) ;
#5740 =( REPRESENTATION_RELATIONSHIP ('NONE','NONE', #12019, #182 ) REPRESENTATION_RELATIONSHIP_WITH_TRANSFORMATION ( #10982 )SHAPE_REPRESENTATION_RELATIONSHIP( ) );
#5741 = CARTESIAN_POINT ( 'NONE',  ( -229.7396143013220637, -4.939964479293777799, -10.94242647241850186 ) ) ;
#5742 = ORIENTED_EDGE ( 'NONE', *, *, #8425, .F. ) ;
#5743 = ORIENTED_EDGE ( 'NONE', *, *, #1850, .T. ) ;
#5744 = CIRCLE ( 'NONE', #1489, 240.2352941176469869 ) ;
#5745 = DIRECTION ( 'NONE',  ( 1.000000000000000000, -0.000000000000000000, 1.224646799147353207E-16 ) ) ;
#5746 = DIRECTION ( 'NONE',  ( 0.000000000000000000, -1.000000000000000000, 0.000000000000000000 ) ) ;
#5747 = AXIS2_PLACEMENT_3D ( 'NONE', #4439, #6393, #4313 ) ;
#5748 = CARTESIAN_POINT ( 'NONE',  ( -196.4640694359484883, 20.79694577636040265, -172.3268284091419957 ) ) ;
#5749 = FACE_OUTER_BOUND ( 'NONE', #1907, .T. ) ;
#5750 = DIRECTION ( 'NONE',  ( -0.9396926207859058744, 0.000000000000000000, -0.3420201433256757628 ) ) ;
#5751 = CARTESIAN_POINT ( 'NONE',  ( 122.2593324768334071, 19.00000000000000000, -168.2755348299895104 ) ) ;
#5752 = DIRECTION ( 'NONE',  ( -0.000000000000000000, -1.000000000000000000, 0.000000000000000000 ) ) ;
#5753 = AXIS2_PLACEMENT_3D ( 'NONE', #2334, #7470, #8540 ) ;
#5754 = EDGE_CURVE ( 'NONE', #171, #8155, #7803, .T. ) ;
#5755 = ORIENTED_EDGE ( 'NONE', *, *, #2712, .F. ) ;
#5756 = AXIS2_PLACEMENT_3D ( 'NONE', #5534, #9592, #477 ) ;
#5757 = CARTESIAN_POINT ( 'NONE',  ( -238.9270525380257197, -1.044268033339604829, 11.95485691302340037 ) ) ;
#5758 = VERTEX_POINT ( 'NONE', #7010 ) ;
#5759 = ORIENTED_EDGE ( 'NONE', *, *, #4966, .F. ) ;
#5760 = EDGE_CURVE ( 'NONE', #5526, #9991, #12875, .T. ) ;
#5761 = CARTESIAN_POINT ( 'NONE',  ( 178.2104428091926138, 20.08915143297736350, 190.2689011420771408 ) ) ;
#5762 = VERTEX_POINT ( 'NONE', #11001 ) ;
#5763 = CIRCLE ( 'NONE', #5116, 6.500000000000005329 ) ;
#5764 = DIRECTION ( 'NONE',  ( 0.000000000000000000, 0.7071067811865570096, 0.7071067811865380248 ) ) ;
#5765 = CARTESIAN_POINT ( 'NONE',  ( 238.9937144808761502, -0.3120165755701557186, -3.486321029136065786 ) ) ;
#5766 = CARTESIAN_POINT ( 'NONE',  ( -260.5542428346390125, 20.08915143307225648, 17.05314194216809653 ) ) ;
#5767 = ORIENTED_EDGE ( 'NONE', *, *, #2955, .T. ) ;
#5768 = FACE_OUTER_BOUND ( 'NONE', #9200, .T. ) ;
#5769 = EDGE_LOOP ( 'NONE', ( #10987, #7450, #12514, #4175 ) ) ;
#5770 = DIRECTION ( 'NONE',  ( -0.4503334343941691187, -0.7071067811865280328, -0.5451603414288131999 ) ) ;
#5771 = ORIENTED_EDGE ( 'NONE', *, *, #3376, .F. ) ;
#5772 = CARTESIAN_POINT ( 'NONE',  ( -241.3329571118387946, 5.362363067925850935, -10.45502706639501334 ) ) ;
#5773 = EDGE_LOOP ( 'NONE', ( #222, #7318 ) ) ;
#5774 = CIRCLE ( 'NONE', #6638, 6.500000000000005329 ) ;
#5775 = CARTESIAN_POINT ( 'NONE',  ( -249.3500139047620223, -10.59807002899673911, 5.074486595336709094 ) ) ;
#5776 = AXIS2_PLACEMENT_3D ( 'NONE', #8395, #2382, #4568 ) ;
#5777 = CARTESIAN_POINT ( 'NONE',  ( 222.8706404512946904, 0.000000000000000000, 0.000000000000000000 ) ) ;
#5778 = DIRECTION ( 'NONE',  ( 0.000000000000000000, -1.000000000000000000, 0.000000000000000000 ) ) ;
#5779 = DIRECTION ( 'NONE',  ( 0.6368676505102708330, 0.000000000000000000, 0.7709731485165535192 ) ) ;
#5780 = CARTESIAN_POINT ( 'NONE',  ( -229.7197566492325222, 3.060063085356466317, -11.35103441395172119 ) ) ;
#5781 = AXIS2_PLACEMENT_3D ( 'NONE', #3225, #8245, #6851 ) ;
#5782 = CARTESIAN_POINT ( 'NONE',  ( -151.8458048843648101, 20.08915143297736705, 211.9058003148604143 ) ) ;
#5783 = CARTESIAN_POINT ( 'NONE',  ( -243.5050917946769857, -7.747614400781110966, 9.163721889611487370 ) ) ;
#5784 = VERTEX_POINT ( 'NONE', #10994 ) ;
#5785 = CARTESIAN_POINT ( 'NONE',  ( -239.6697886797803960, 1.970929118521804968, -11.83704280435266298 ) ) ;
#5786 = CONTEXT_DEPENDENT_SHAPE_REPRESENTATION ( #5047, #7351 ) ;
#5787 = ORIENTED_EDGE ( 'NONE', *, *, #9412, .T. ) ;
#5788 = CARTESIAN_POINT ( 'NONE',  ( -229.6989731110666924, 2.477381075173155978, 11.76526715247366894 ) ) ;
#5789 = EDGE_CURVE ( 'NONE', #9651, #12366, #2793, .T. ) ;
#5790 = VERTEX_POINT ( 'NONE', #11944 ) ;
#5791 = ORIENTED_EDGE ( 'NONE', *, *, #8978, .F. ) ;
#5792 = CARTESIAN_POINT ( 'NONE',  ( -249.2564709991243603, -10.48830713239226320, -5.296988132951380379 ) ) ;
#5793 = ORIENTED_EDGE ( 'NONE', *, *, #8650, .T. ) ;
#5794 = CARTESIAN_POINT ( 'NONE',  ( 17.10461161519311091, 20.55460285116648933, 261.3381329044966606 ) ) ;
#5795 = DIRECTION ( 'NONE',  ( 0.000000000000000000, 0.7071067811865480168, 0.7071067811865470176 ) ) ;
#5796 = B_SPLINE_CURVE_WITH_KNOTS ( 'NONE', 3,
 ( #12607, #3471, #9726, #7546, #5538, #4660, #12675, #7669, #8740, #7606, #7482, #6615, #5609, #3331, #11484, #10481, #1350, #5416, #9480, #12542, #2789, #6009, #11816, #3666, #2856, #9822, #4997, #9007, #748, #8870, #4798, #11940, #4729, #1936, #806, #6875, #3931, #12934, #3800, #7867, #10937, #8806, #7737, #1813, #5877, #9931, #1671, #4867, #12870, #10066, #5741, #8007, #2661, #3865, #2720, #7800, #11874, #4931, #5810 ),
 .UNSPECIFIED., .F., .F.,
 ( 4, 2, 2, 2, 2, 2, 2, 2, 1, 2, 2, 1, 2, 2, 1, 2, 2, 2, 2, 2, 2, 2, 2, 2, 2, 2, 2, 2, 2, 2, 4 ),
 ( 0.000000000000000000, 0.06249999999999980571, 0.1249999999999996669, 0.1874999999999995282, 0.2187499999999995282, 0.2499999999999995559, 0.2812499999999995559, 0.3124999999999995559, 0.3437499999999996114, 0.3593749999999996114, 0.3749999999999996114, 0.4062499999999996114, 0.4218749999999996114, 0.4374999999999996114, 0.4687499999999997224, 0.4843749999999997780, 0.4999999999999997780, 0.5312499999999997780, 0.5624999999999997780, 0.5937499999999997780, 0.6249999999999997780, 0.6875000000000000000, 0.7500000000000001110, 0.7812500000000002220, 0.8125000000000002220, 0.8437500000000002220, 0.8750000000000002220, 0.9062500000000003331, 0.9218750000000002220, 0.9375000000000002220, 1.000000000000000000 ),
 .UNSPECIFIED. ) ;
#5797 = LINE ( 'NONE', #4714, #10621 ) ;
#5798 = CIRCLE ( 'NONE', #688, 250.1999999999999602 ) ;
#5799 = DIRECTION ( 'NONE',  ( 0.000000000000000000, -1.000000000000000000, 0.000000000000000000 ) ) ;
#5800 = CIRCLE ( 'NONE', #10493, 4.500000000000000000 ) ;
#5801 = LINE ( 'NONE', #2590, #3555 ) ;
#5802 = CARTESIAN_POINT ( 'NONE',  ( 0.000000000000000000, 30.00000000000000000, -208.0000000000000000 ) ) ;
#5803 = DIRECTION ( 'NONE',  ( -0.6820219226572428184, 0.5538822189107471816, -0.4775568914688856914 ) ) ;
#5804 = CARTESIAN_POINT ( 'NONE',  ( 0.000000000000000000, 18.00000000000000000, -214.5000000000000000 ) ) ;
#5805 = VECTOR ( 'NONE', #7937, 1000.000000000000000 ) ;
#5806 = EDGE_CURVE ( 'NONE', #8008, #3549, #7142, .T. ) ;
#5807 = PRODUCT_DEFINITION_SHAPE ( 'NONE', 'NONE',  #13155 ) ;
#5808 = CARTESIAN_POINT ( 'NONE',  ( -249.7843163504555548, 11.60707272978753757, 1.827122155623386091 ) ) ;
#5809 = CARTESIAN_POINT ( 'NONE',  ( -240.3908911751984760, -3.583360156735717617, -11.45287536844211473 ) ) ;
#5810 = CARTESIAN_POINT ( 'NONE',  ( -229.6889200636375108, -1.000000000000000000, -11.95826074310140008 ) ) ;
#5811 = EDGE_LOOP ( 'NONE', ( #9920, #2747, #5072, #2933 ) ) ;
#5812 = VERTEX_POINT ( 'NONE', #9801 ) ;
#5813 = CARTESIAN_POINT ( 'NONE',  ( -130.5770120874175859, 20.08915143279216764, 226.1171533172259842 ) ) ;
#5814 = DIRECTION ( 'NONE',  ( 0.000000000000000000, 1.000000000000000000, 0.000000000000000000 ) ) ;
#5815 = EDGE_CURVE ( 'NONE', #6766, #9399, #6078, .T. ) ;
#5816 = EDGE_CURVE ( 'NONE', #7165, #11682, #3726, .T. ) ;
#5817 = AXIS2_PLACEMENT_3D ( 'NONE', #10809, #3609, #9604 ) ;
#5818 = CARTESIAN_POINT ( 'NONE',  ( 196.8887528220037950, 20.55460285134802589, -172.6991790960863966 ) ) ;
#5819 = CARTESIAN_POINT ( 'NONE',  ( -290.6841825403030839, -19.00000000000000000, -27.68945685411394919 ) ) ;
#5820 = DIRECTION ( 'NONE',  ( -0.2588190451025111916, 0.000000000000000000, -0.9659258262890708657 ) ) ;
#5821 = AXIS2_PLACEMENT_3D ( 'NONE', #2356, #11493, #2283 ) ;
#5822 = CARTESIAN_POINT ( 'NONE',  ( -122.2593324768359935, 30.00000000000000000, -174.7755348299880040 ) ) ;
#5823 = AXIS2_PLACEMENT_3D ( 'NONE', #8163, #11289, #12227 ) ;
#5824 = DIRECTION ( 'NONE',  ( 0.4503334343941574613, 0.7071067811865460184, 0.5451603414287994331 ) ) ;
#5825 = VERTEX_POINT ( 'NONE', #943 ) ;
#5826 = CARTESIAN_POINT ( 'NONE',  ( -239.9450917581429792, -2.156506209390995021, 11.80463811257499884 ) ) ;
#5827 = ORIENTED_EDGE ( 'NONE', *, *, #8326, .F. ) ;
#5828 = ORIENTED_EDGE ( 'NONE', *, *, #4967, .T. ) ;
#5829 = VECTOR ( 'NONE', #4552, 1000.000000000000000 ) ;
#5830 = CONICAL_SURFACE ( 'NONE', #3476, 5.500000000000007994, 0.7853981633974461696 ) ;
#5831 = B_SPLINE_CURVE_WITH_KNOTS ( 'NONE', 3,
 ( #5616, #10746, #1683, #7876 ),
 .UNSPECIFIED., .F., .F.,
 ( 4, 4 ),
 ( 0.000000000000000000, 1.000000000000000000 ),
 .UNSPECIFIED. ) ;
#5832 = CARTESIAN_POINT ( 'NONE',  ( -250.0000000000000000, 1.000000000000000000, 11.95826074310140008 ) ) ;
#5833 = ORIENTED_EDGE ( 'NONE', *, *, #3491, .F. ) ;
#5834 = AXIS2_PLACEMENT_3D ( 'NONE', #539, #7469, #11607 ) ;
#5835 = EDGE_CURVE ( 'NONE', #90, #953, #6719, .T. ) ;
#5836 = FACE_OUTER_BOUND ( 'NONE', #8972, .T. ) ;
#5837 = EDGE_CURVE ( 'NONE', #5907, #3975, #4687, .T. ) ;
#5838 = CARTESIAN_POINT ( 'NONE',  ( 71.82423009839129691, 30.00000000000000000, -197.3354503650404865 ) ) ;
#5839 = DIRECTION ( 'NONE',  ( -0.000000000000000000, 1.000000000000000000, 0.000000000000000000 ) ) ;
#5840 = PRODUCT_DEFINITION_SHAPE ( 'NONE', 'NONE',  #13041 ) ;
#5841 = CIRCLE ( 'NONE', #5178, 195.0000000000000000 ) ;
#5842 = ADVANCED_FACE ( 'NONE', ( #4733 ), #11076, .T. ) ;
#5843 = VERTEX_POINT ( 'NONE', #6005 ) ;
#5844 = CARTESIAN_POINT ( 'NONE',  ( 0.000000000000000000, 29.00000000000000000, 0.000000000000000000 ) ) ;
#5845 = VERTEX_POINT ( 'NONE', #6869 ) ;
#5846 = CARTESIAN_POINT ( 'NONE',  ( -238.7779969860605718, 0.6784773152999695744, 11.73519575009920857 ) ) ;
#5847 = EDGE_LOOP ( 'NONE', ( #6076, #8953, #8968, #4579 ) ) ;
#5848 = AXIS2_PLACEMENT_3D ( 'NONE', #2337, #10267, #12410 ) ;
#5849 = FACE_OUTER_BOUND ( 'NONE', #12506, .T. ) ;
#5850 = LINE ( 'NONE', #10102, #31 ) ;
#5851 = CARTESIAN_POINT ( 'NONE',  ( -249.8000249158748716, -12.00052859682465112, 0.5791969794071849531 ) ) ;
#5852 = CARTESIAN_POINT ( 'NONE',  ( 132.6365829178909621, -28.60000000000000142, -260.1259780660157048 ) ) ;
#5853 = CARTESIAN_POINT ( 'NONE',  ( -258.4638482596386098, 20.08915143297737060, -34.02434144668580274 ) ) ;
#5854 = CARTESIAN_POINT ( 'NONE',  ( -242.4607547069787188, -6.794574167113599295, 9.891349723532682603 ) ) ;
#5855 = CARTESIAN_POINT ( 'NONE',  ( -239.0946434567509300, 1.343932711761059329, -11.92448114280328575 ) ) ;
#5856 = ORIENTED_EDGE ( 'NONE', *, *, #3871, .T. ) ;
#5857 = DIRECTION ( 'NONE',  ( 0.6368676505102707219, 0.000000000000000000, 0.7709731485165536302 ) ) ;
#5858 = ITEM_DEFINED_TRANSFORMATION ( 'NONE', 'NONE', #3624,  #805 ) ;
#5859 = VECTOR ( 'NONE', #12727, 1000.000000000000114 ) ;
#5860 = EDGE_LOOP ( 'NONE', ( #3751, #2734, #7671, #22 ) ) ;
#5861 = VERTEX_POINT ( 'NONE', #3788 ) ;
#5862 = FACE_OUTER_BOUND ( 'NONE', #2877, .T. ) ;
#5863 = EDGE_LOOP ( 'NONE', ( #5624, #8992, #1633, #6370 ) ) ;
#5864 = CARTESIAN_POINT ( 'NONE',  ( 261.3381329044966606, 20.55460285106647689, 17.10461161501256555 ) ) ;
#5865 = DIRECTION ( 'NONE',  ( 0.000000000000000000, 0.000000000000000000, -1.000000000000000000 ) ) ;
#5866 = DIRECTION ( 'NONE',  ( 0.6368676505102707219, 0.000000000000000000, 0.7709731485165536302 ) ) ;
#5867 = ADVANCED_FACE ( 'NONE', ( #8137 ), #964, .T. ) ;
#5868 = DIRECTION ( 'NONE',  ( 0.000000000000000000, -1.000000000000000000, 0.000000000000000000 ) ) ;
#5869 = CIRCLE ( 'NONE', #7002, 6.500000000000005329 ) ;
#5870 = CARTESIAN_POINT ( 'NONE',  ( -239.5361044668159991, -1.848645179572815156, 11.60366368868215758 ) ) ;
#5871 = SURFACE_STYLE_USAGE ( .BOTH. , #2781 ) ;
#5872 = DIRECTION ( 'NONE',  ( -0.6427876096865430267, 0.000000000000000000, 0.7660444431189749048 ) ) ;
#5873 = CYLINDRICAL_SURFACE ( 'NONE', #5633, 254.0000000000000000 ) ;
#5874 = CONTEXT_DEPENDENT_SHAPE_REPRESENTATION ( #2153, #4726 ) ;
#5875 = CARTESIAN_POINT ( 'NONE',  ( -249.7982158291746941, 11.73176039496360445, -0.7224695577198212426 ) ) ;
#5876 =( REPRESENTATION_RELATIONSHIP ('NONE','NONE', #12019, #5191 ) REPRESENTATION_RELATIONSHIP_WITH_TRANSFORMATION ( #3380 )SHAPE_REPRESENTATION_RELATIONSHIP( ) );
#5877 = CARTESIAN_POINT ( 'NONE',  ( -229.8176334827029734, -7.760374230956414543, -9.160644146514997033 ) ) ;
#5878 = ORIENTED_EDGE ( 'NONE', *, *, #8334, .T. ) ;
#5879 = ORIENTED_EDGE ( 'NONE', *, *, #12750, .T. ) ;
#5880 = AXIS2_PLACEMENT_3D ( 'NONE', #877, #5002, #1941 ) ;
#5881 = CARTESIAN_POINT ( 'NONE',  ( 0.000000000000000000, -2.957522019940860139E-14, 0.000000000000000000 ) ) ;
#5882 = DIRECTION ( 'NONE',  ( -0.6368676505102700558, 0.000000000000000000, -0.7709731485165541853 ) ) ;
#5883 = ADVANCED_FACE ( 'NONE', ( #2912 ), #9678, .F. ) ;
#5884 = ADVANCED_FACE ( 'NONE', ( #8937 ), #1174, .F. ) ;
#5885 = CARTESIAN_POINT ( 'NONE',  ( -159.0697709846024850, 20.79694577629653551, -207.3438552932539949 ) ) ;
#5886 = CYLINDRICAL_SURFACE ( 'NONE', #2403, 5.500000000000007994 ) ;
#5887 = CARTESIAN_POINT ( 'NONE',  ( 0.000000000000000000, 0.000000000000000000, 0.000000000000000000 ) ) ;
#5888 = CARTESIAN_POINT ( 'NONE',  ( 0.000000000000000000, 0.000000000000000000, 0.000000000000000000 ) ) ;
#5889 = EDGE_LOOP ( 'NONE', ( #4824, #7154, #8687, #9055 ) ) ;
#5890 = EDGE_CURVE ( 'NONE', #10191, #552, #11397, .T. ) ;
#5891 = CARTESIAN_POINT ( 'NONE',  ( 220.3999999999999773, 0.9998057603070324983, -0.01970892327970869343 ) ) ;
#5892 = CARTESIAN_POINT ( 'NONE',  ( -239.6107305401175154, -1.923727060014592372, 11.84479882370300352 ) ) ;
#5893 = VERTEX_POINT ( 'NONE', #12199 ) ;
#5894 = ORIENTED_EDGE ( 'NONE', *, *, #5890, .F. ) ;
#5895 = ORIENTED_EDGE ( 'NONE', *, *, #2638, .T. ) ;
#5896 = DIRECTION ( 'NONE',  ( 0.000000000000000000, 0.9998057603070480415, -0.01970892327970899874 ) ) ;
#5897 = CARTESIAN_POINT ( 'NONE',  ( -226.1171533162824971, 20.08915143300168893, 130.5770120869439950 ) ) ;
#5898 = CARTESIAN_POINT ( 'NONE',  ( 71.82423009839129691, 30.00000000000000000, 203.8354503650404865 ) ) ;
#5899 = CARTESIAN_POINT ( 'NONE',  ( 0.000000000000000000, -20.00000000000000000, -231.0000000000000000 ) ) ;
#5900 = AXIS2_PLACEMENT_3D ( 'NONE', #1355, #6356, #5353 ) ;
#5901 = ORIENTED_EDGE ( 'NONE', *, *, #11244, .F. ) ;
#5902 = DIRECTION ( 'NONE',  ( 1.000000000000000000, 0.000000000000000000, 0.000000000000000000 ) ) ;
#5903 = ADVANCED_FACE ( 'NONE', ( #3988 ), #11062, .T. ) ;
#5904 = ORIENTED_EDGE ( 'NONE', *, *, #9245, .T. ) ;
#5905 = ADVANCED_FACE ( 'NONE', ( #8001 ), #9903, .T. ) ;
#5906 = CARTESIAN_POINT ( 'NONE',  ( -247.1684828253810906, 9.630976095903571732, -6.736800400388656129 ) ) ;
#5907 = VERTEX_POINT ( 'NONE', #3051 ) ;
#5908 = AXIS2_PLACEMENT_3D ( 'NONE', #1642, #7906, #11848 ) ;
#5909 = DIRECTION ( 'NONE',  ( 0.000000000000000000, 0.000000000000000000, 1.000000000000000000 ) ) ;
#5910 = DIRECTION ( 'NONE',  ( 0.000000000000000000, 0.000000000000000000, 1.000000000000000000 ) ) ;
#5911 = MANIFOLD_SOLID_BREP ( 'NONE', #7524 ) ;
#5912 = DIRECTION ( 'NONE',  ( 0.000000000000000000, -0.7071067811865480168, -0.7071067811865470176 ) ) ;
#5913 = FACE_OUTER_BOUND ( 'NONE', #4777, .T. ) ;
#5914 = FACE_BOUND ( 'NONE', #8022, .T. ) ;
#5915 = PRODUCT_DEFINITION_SHAPE ( 'NONE', 'NONE',  #13160 ) ;
#5916 = CARTESIAN_POINT ( 'NONE',  ( -240.5954930648636036, -4.058997395512141004, 11.29299565151879570 ) ) ;
#5917 = AXIS2_PLACEMENT_3D ( 'NONE', #6575, #1438, #5500 ) ;
#5918 = CARTESIAN_POINT ( 'NONE',  ( -239.5355864646326154, 1.859542262448960148, -11.85503689126069915 ) ) ;
#5919 =( REPRESENTATION_RELATIONSHIP ('NONE','NONE', #12019, #182 ) REPRESENTATION_RELATIONSHIP_WITH_TRANSFORMATION ( #9178 )SHAPE_REPRESENTATION_RELATIONSHIP( ) );
#5920 = ORIENTED_EDGE ( 'NONE', *, *, #2684, .F. ) ;
#5921 = CARTESIAN_POINT ( 'NONE',  ( -238.7194017472469341, -0.2080061402095525758, -11.74814821798330478 ) ) ;
#5922 = VERTEX_POINT ( 'NONE', #4856 ) ;
#5923 = EDGE_CURVE ( 'NONE', #12436, #9350, #5210, .T. ) ;
#5924 = ORIENTED_EDGE ( 'NONE', *, *, #1182, .F. ) ;
#5925 = CARTESIAN_POINT ( 'NONE',  ( -249.2624683436029898, -10.49496574118427716, -5.283769350921994068 ) ) ;
#5926 = EDGE_LOOP ( 'NONE', ( #3918, #660, #9217, #6011 ) ) ;
#5927 = AXIS2_PLACEMENT_3D ( 'NONE', #1212, #3199, #7212 ) ;
#5928 = CARTESIAN_POINT ( 'NONE',  ( -67.76049180241520276, 20.55460285097757378, 252.9796497716870078 ) ) ;
#5929 = FACE_OUTER_BOUND ( 'NONE', #10813, .T. ) ;
#5930 = LINE ( 'NONE', #4852, #1469 ) ;
#5931 = CARTESIAN_POINT ( 'NONE',  ( -233.0000000000000000, -1.000000000000000000, 11.95826074310140008 ) ) ;
#5932 = CARTESIAN_POINT ( 'NONE',  ( -246.5647187084086625, 9.432500522705552726, 7.418392397108976688 ) ) ;
#5933 =( REPRESENTATION_RELATIONSHIP ('NONE','NONE', #12019, #182 ) REPRESENTATION_RELATIONSHIP_WITH_TRANSFORMATION ( #3628 )SHAPE_REPRESENTATION_RELATIONSHIP( ) );
#5934 = DIRECTION ( 'NONE',  ( 0.000000000000000000, -0.9998057603070481525, 0.01970892327970899874 ) ) ;
#5935 = MANIFOLD_SOLID_BREP ( 'NONE', #4530 ) ;
#5936 = CARTESIAN_POINT ( 'NONE',  ( 20.92562098022577644, -138.4705547276867321, -36.24423871767961458 ) ) ;
#5937 = AXIS2_PLACEMENT_3D ( 'NONE', #2476, #10347, #2278 ) ;
#5938 = AXIS2_PLACEMENT_3D ( 'NONE', #2378, #6453, #9383 ) ;
#5939 = CARTESIAN_POINT ( 'NONE',  ( 27.68945685411497593, -19.00000000000000000, -290.6841825403026291 ) ) ;
#5940 = AXIS2_PLACEMENT_3D ( 'NONE', #6493, #1481, #9535 ) ;
#5941 = CONTEXT_DEPENDENT_SHAPE_REPRESENTATION ( #11983, #6872 ) ;
#5942 = AXIS2_PLACEMENT_3D ( 'NONE', #4922, #9857, #8996 ) ;
#5943 = LINE ( 'NONE', #1743, #6230 ) ;
#5944 = ORIENTED_EDGE ( 'NONE', *, *, #6818, .T. ) ;
#5945 = AXIS2_PLACEMENT_3D ( 'NONE', #8603, #12662, #6864 ) ;
#5946 = EDGE_LOOP ( 'NONE', ( #7241, #1067, #3362, #6220 ) ) ;
#5947 = LINE ( 'NONE', #3996, #2092 ) ;
#5948 = AXIS2_PLACEMENT_3D ( 'NONE', #6396, #1516, #11655 ) ;
#5949 = CARTESIAN_POINT ( 'NONE',  ( -197.8197553893909912, 30.00000000000000000, 64.27553482999130097 ) ) ;
#5950 = DIRECTION ( 'NONE',  ( -0.000000000000000000, -1.000000000000000000, 0.000000000000000000 ) ) ;
#5951 = PRESENTATION_LAYER_ASSIGNMENT (  '', '', ( #32 ) ) ;
#5952 = DIRECTION ( 'NONE',  ( -0.1736481776669241417, 0.000000000000000000, -0.9848077530122091305 ) ) ;
#5953 = CARTESIAN_POINT ( 'NONE',  ( -244.9693137076198752, -8.715706976269279593, 7.881056910973075702 ) ) ;
#5954 = ORIENTED_EDGE ( 'NONE', *, *, #657, .F. ) ;
#5955 = EDGE_CURVE ( 'NONE', #7121, #8160, #6083, .T. ) ;
#5956 = CARTESIAN_POINT ( 'NONE',  ( 197.8197553893920144, 18.00000000000000000, 70.77553482998851564 ) ) ;
#5957 = EDGE_CURVE ( 'NONE', #366, #2076, #2026, .T. ) ;
#5958 = CIRCLE ( 'NONE', #4883, 5.500000000000005329 ) ;
#5959 = MANIFOLD_SOLID_BREP ( 'NONE', #6257 ) ;
#5960 = CARTESIAN_POINT ( 'NONE',  ( -239.1644449915108908, -1.447449310967494629, 11.91236063150040003 ) ) ;
#5961 = ORIENTED_EDGE ( 'NONE', *, *, #10627, .F. ) ;
#5962 = ORIENTED_EDGE ( 'NONE', *, *, #9547, .T. ) ;
#5963 = PRODUCT_DEFINITION_CONTEXT ( 'detailed design', #8893, 'design' ) ;
#5964 = DIRECTION ( 'NONE',  ( 0.000000000000000000, -0.7071067811865489050, -0.7071067811865460184 ) ) ;
#5965 = DIRECTION ( 'NONE',  ( -0.4503334343941582940, -0.7071067811865450192, -0.5451603414288000993 ) ) ;
#5966 = CARTESIAN_POINT ( 'NONE',  ( -249.0998459876556979, 10.33180199737826577, 5.596503889598144710 ) ) ;
#5967 = PRODUCT_RELATED_PRODUCT_CATEGORY ( 'part', '', ( #115 ) ) ;
#5968 = CARTESIAN_POINT ( 'NONE',  ( 17.09264059789564172, 19.96883746058902176, -261.1558126970361400 ) ) ;
#5969 = CIRCLE ( 'NONE', #217, 5.499999999999986677 ) ;
#5970 = CARTESIAN_POINT ( 'NONE',  ( -238.7877125588677529, -0.6581212608206794545, -11.98194713172116543 ) ) ;
#5971 = CARTESIAN_POINT ( 'NONE',  ( 220.9845196385168435, -30.00000000000000000, -190.9766794143566528 ) ) ;
#5972 = ORIENTED_EDGE ( 'NONE', *, *, #9889, .T. ) ;
#5973 = CARTESIAN_POINT ( 'NONE',  ( 71.82423009839129691, 30.00000000000000000, -197.3354503650404865 ) ) ;
#5974 = ORIENTED_EDGE ( 'NONE', *, *, #3004, .F. ) ;
#5975 = CARTESIAN_POINT ( 'NONE',  ( -246.1720478471803517, 9.282004956765195658, -7.205195109033324385 ) ) ;
#5976 = ORIENTED_EDGE ( 'NONE', *, *, #4801, .F. ) ;
#5977 = CARTESIAN_POINT ( 'NONE',  ( 130.7196491263533744, -20.00000000000000000, -200.0834159351620656 ) ) ;
#5978 = AXIS2_PLACEMENT_3D ( 'NONE', #11612, #4524, #6611 ) ;
#5979 = DIRECTION ( 'NONE',  ( 0.6368676505102695007, 0.000000000000000000, 0.7709731485165545184 ) ) ;
#5980 = CARTESIAN_POINT ( 'NONE',  ( 240.3826708216974737, 2.772967769358989809, -2.135567781667440102 ) ) ;
#5981 = EDGE_CURVE ( 'NONE', #4180, #2618, #7328, .T. ) ;
#5982 = CARTESIAN_POINT ( 'NONE',  ( 0.000000000000000000, 0.000000000000000000, -249.7999999999999829 ) ) ;
#5983 = EDGE_CURVE ( 'NONE', #9116, #12435, #10543, .T. ) ;
#5984 = DIRECTION ( 'NONE',  ( 0.4503334343941574613, 0.7071067811865460184, 0.5451603414287994331 ) ) ;
#5985 = CARTESIAN_POINT ( 'NONE',  ( -244.8752249710313436, -8.669362157865133867, 8.297136228535620717 ) ) ;
#5986 = CARTESIAN_POINT ( 'NONE',  ( -239.6279820821901296, 1.937806669454118946, -11.84250614158974280 ) ) ;
#5987 = UNCERTAINTY_MEASURE_WITH_UNIT (LENGTH_MEASURE( 1.000000000000000082E-05 ), #867, 'distance_accuracy_value', 'NONE');
#5988 = CONTEXT_DEPENDENT_SHAPE_REPRESENTATION ( #2503, #9753 ) ;
#5989 = ORIENTED_EDGE ( 'NONE', *, *, #6531, .T. ) ;
#5990 = FACE_OUTER_BOUND ( 'NONE', #6022, .T. ) ;
#5991 = EDGE_CURVE ( 'NONE', #8275, #7222, #12792, .T. ) ;
#5992 = VERTEX_POINT ( 'NONE', #1128 ) ;
#5993 = VERTEX_POINT ( 'NONE', #1646 ) ;
#5994 = CARTESIAN_POINT ( 'NONE',  ( -248.8285144558357445, -10.12619208585344133, 5.960099103772717122 ) ) ;
#5995 = ORIENTED_EDGE ( 'NONE', *, *, #5705, .T. ) ;
#5996 = AXIS2_PLACEMENT_3D ( 'NONE', #12243, #3966, #2037 ) ;
#5997 = CARTESIAN_POINT ( 'NONE',  ( 34.20858920311310669, 20.55460285062568815, 259.6535381495587558 ) ) ;
#5998 = CARTESIAN_POINT ( 'NONE',  ( -246.1739743501388773, 9.287690275995652556, -7.598953578997135416 ) ) ;
#5999 = CARTESIAN_POINT ( 'NONE',  ( 0.000000000000000000, 0.000000000000000000, 0.000000000000000000 ) ) ;
#6000 = CARTESIAN_POINT ( 'NONE',  ( 227.3999999999999773, -0.1281080013181084831, -6.498737441995811714 ) ) ;
#6001 = CIRCLE ( 'NONE', #6206, 8.000000000000007105 ) ;
#6002 = CARTESIAN_POINT ( 'NONE',  ( -239.3015193013782209, -1.606994374921540736, -11.63956803099216586 ) ) ;
#6003 = EDGE_CURVE ( 'NONE', #7702, #1100, #4788, .T. ) ;
#6004 = CARTESIAN_POINT ( 'NONE',  ( -243.6963328790136245, 7.900314958675304311, 9.035065364342628413 ) ) ;
#6005 = CARTESIAN_POINT ( 'NONE',  ( 122.2593324768334071, 18.00000000000000000, -161.7755348299894820 ) ) ;
#6006 = DIRECTION ( 'NONE',  ( 0.4775568914688745337, 0.5538822189107472926, 0.6820219226572509230 ) ) ;
#6007 = CARTESIAN_POINT ( 'NONE',  ( -221.6213872890270977, -19.00000000000000000, 190.2057062658400923 ) ) ;
#6008 = EDGE_CURVE ( 'NONE', #204, #3634, #541, .T. ) ;
#6009 = CARTESIAN_POINT ( 'NONE',  ( -229.9741363928493172, -11.49453502056800858, 3.481240219726035701 ) ) ;
#6010 = ORIENTED_EDGE ( 'NONE', *, *, #11781, .T. ) ;
#6011 = ORIENTED_EDGE ( 'NONE', *, *, #8650, .F. ) ;
#6012 = VECTOR ( 'NONE', #118, 1000.000000000000000 ) ;
#6013 = DIRECTION ( 'NONE',  ( -0.000000000000000000, -1.000000000000000000, 0.000000000000000000 ) ) ;
#6014 = CARTESIAN_POINT ( 'NONE',  ( 0.000000000000000000, 9.830508068699479907, 248.1666666666505137 ) ) ;
#6015 = DIRECTION ( 'NONE',  ( 0.000000000000000000, -0.7071067811865489050, -0.7071067811865460184 ) ) ;
#6016 = CIRCLE ( 'NONE', #11558, 6.500000000000005329 ) ;
#6017 = CARTESIAN_POINT ( 'NONE',  ( -197.8197553893924976, 29.00000000000000000, -58.77553482998720114 ) ) ;
#6018 = DIRECTION ( 'NONE',  ( 0.000000000000000000, 1.000000000000000000, 0.000000000000000000 ) ) ;
#6019 = DIRECTION ( 'NONE',  ( -0.2154914511802873689, 0.5538822189107472926, 0.8042250444015787147 ) ) ;
#6020 = AXIS2_PLACEMENT_3D ( 'NONE', #7891, #6164, #1092 ) ;
#6021 = CARTESIAN_POINT ( 'NONE',  ( -243.1145437064502062, -7.410518230721312882, 9.118492839119728188 ) ) ;
#6022 = EDGE_LOOP ( 'NONE', ( #1622, #8019, #7185, #4732, #1441 ) ) ;
#6023 = AXIS2_PLACEMENT_3D ( 'NONE', #8149, #12214, #11205 ) ;
#6024 = FACE_OUTER_BOUND ( 'NONE', #9774, .T. ) ;
#6025 = CARTESIAN_POINT ( 'NONE',  ( -239.5624944382587103, -1.883403856151246947, 11.85129291893081138 ) ) ;
#6026 = EDGE_LOOP ( 'NONE', ( #9311, #6688, #9986, #2969 ) ) ;
#6027 = EDGE_LOOP ( 'NONE', ( #1797, #9898 ) ) ;
#6028 = CARTESIAN_POINT ( 'NONE',  ( 233.5975020798683204, -2.999417280921144346, 0.05912676983912736745 ) ) ;
#6029 = CARTESIAN_POINT ( 'NONE',  ( 0.000000000000000000, -20.00000000000000000, 0.000000000000000000 ) ) ;
#6030 = PRODUCT_DEFINITION_SHAPE ( 'NONE', 'NONE',  #13114 ) ;
#6031 = CIRCLE ( 'NONE', #12626, 251.1999999999999886 ) ;
#6032 = CARTESIAN_POINT ( 'NONE',  ( -249.6727234477378090, 11.17009475772721494, 3.645778574476101763 ) ) ;
#6033 = AXIS2_PLACEMENT_3D ( 'NONE', #1838, #10766, #8696 ) ;
#6034 = ADVANCED_FACE ( 'NONE', ( #7525 ), #5218, .F. ) ;
#6035 = CARTESIAN_POINT ( 'NONE',  ( 258.8746690706130380, 20.08915143329827657, -34.10614053547809732 ) ) ;
#6036 = CARTESIAN_POINT ( 'NONE',  ( -238.8086796927654802, -0.7305208660282929145, -11.97777837065560114 ) ) ;
#6037 = CARTESIAN_POINT ( 'NONE',  ( -243.1925160191523219, 7.478514345020445653, 9.062807753481795459 ) ) ;
#6038 = ORIENTED_EDGE ( 'NONE', *, *, #12634, .T. ) ;
#6039 = DIRECTION ( 'NONE',  ( 0.000000000000000000, 1.000000000000000000, 0.000000000000000000 ) ) ;
#6040 = AXIS2_PLACEMENT_3D ( 'NONE', #12498, #10430, #506 ) ;
#6041 = ORIENTED_EDGE ( 'NONE', *, *, #11291, .T. ) ;
#6042 = AXIS2_PLACEMENT_3D ( 'NONE', #3408, #5550, #11629 ) ;
#6043 = CARTESIAN_POINT ( 'NONE',  ( -239.2405902068692569, 1.531671734703150323, 11.64972311196225085 ) ) ;
#6044 = ORIENTED_EDGE ( 'NONE', *, *, #4257, .T. ) ;
#6045 = CARTESIAN_POINT ( 'NONE',  ( -159.3442861576697283, 0.000000000000000000, -192.8974817588416499 ) ) ;
#6046 = DIRECTION ( 'NONE',  ( 0.000000000000000000, 0.000000000000000000, 1.000000000000000000 ) ) ;
#6047 = CYLINDRICAL_SURFACE ( 'NONE', #626, 270.0000000000000000 ) ;
#6048 = EDGE_CURVE ( 'NONE', #8424, #11763, #2868, .T. ) ;
#6049 = DIRECTION ( 'NONE',  ( 0.000000000000000000, 1.000000000000000000, 0.000000000000000000 ) ) ;
#6050 = CONICAL_SURFACE ( 'NONE', #731, 5.500000000000005329, 0.7853981633974461696 ) ;
#6051 = CARTESIAN_POINT ( 'NONE',  ( -233.0000000000000000, 1.469576158976823947E-15, 12.00000000000000000 ) ) ;
#6052 = DIRECTION ( 'NONE',  ( 0.5469441386039890496, 0.000000000000000000, -0.8371691043312220470 ) ) ;
#6053 = CIRCLE ( 'NONE', #9878, 6.499999999999999112 ) ;
#6054 = CARTESIAN_POINT ( 'NONE',  ( -239.4529136937619000, 1.782225492116373600, -11.86690533460318342 ) ) ;
#6055 = CONTEXT_DEPENDENT_SHAPE_REPRESENTATION ( #5919, #8421 ) ;
#6056 = ORIENTED_EDGE ( 'NONE', *, *, #371, .F. ) ;
#6057 = CARTESIAN_POINT ( 'NONE',  ( -239.1331745461246783, -1.386667398511050253, -11.66814598037958461 ) ) ;
#6058 = ORIENTED_EDGE ( 'NONE', *, *, #1829, .F. ) ;
#6059 = CARTESIAN_POINT ( 'NONE',  ( -246.5647187074482645, -9.432500522371258356, -7.418392397481870404 ) ) ;
#6060 = EDGE_CURVE ( 'NONE', #10237, #3272, #8594, .T. ) ;
#6061 = AXIS2_PLACEMENT_3D ( 'NONE', #1240, #12502, #12636 ) ;
#6062 = CARTESIAN_POINT ( 'NONE',  ( 42.46883004693721375, 20.08915143297736705, -257.2112267038639288 ) ) ;
#6063 = ORIENTED_EDGE ( 'NONE', *, *, #7034, .T. ) ;
#6064 = CARTESIAN_POINT ( 'NONE',  ( 115.5625104413773983, 20.79694577638496966, -234.3927740979615066 ) ) ;
#6065 = CARTESIAN_POINT ( 'NONE',  ( -247.9423986615486797, 9.805815554877437279, -6.917079555552443360 ) ) ;
#6066 = FACE_OUTER_BOUND ( 'NONE', #5769, .T. ) ;
#6067 = CARTESIAN_POINT ( 'NONE',  ( -247.4721532363031429, -9.698102445084007428, -6.633777139480653950 ) ) ;
#6068 = CARTESIAN_POINT ( 'NONE',  ( -249.7118339206215012, 9.997999799959989886, 6.636264009214830395 ) ) ;
#6069 = CIRCLE ( 'NONE', #1807, 260.1830065359559967 ) ;
#6070 = CARTESIAN_POINT ( 'NONE',  ( 34.28253040793683937, -138.4705547276867321, -24.00488622054054133 ) ) ;
#6071 = CARTESIAN_POINT ( 'NONE',  ( 0.000000000000000000, -23.50000000000000000, 0.000000000000000000 ) ) ;
#6072 = ITEM_DEFINED_TRANSFORMATION ( 'NONE', 'NONE', #6618,  #805 ) ;
#6073 = EDGE_CURVE ( 'NONE', #2870, #6308, #10553, .T. ) ;
#6074 = ADVANCED_FACE ( 'NONE', ( #4510 ), #3512, .F. ) ;
#6075 = DIRECTION ( 'NONE',  ( 0.000000000000000000, 1.000000000000000000, 0.000000000000000000 ) ) ;
#6076 = ORIENTED_EDGE ( 'NONE', *, *, #6958, .T. ) ;
#6077 = ORIENTED_EDGE ( 'NONE', *, *, #6698, .F. ) ;
#6078 = CIRCLE ( 'NONE', #7990, 3.823498366181860231 ) ;
#6079 = CARTESIAN_POINT ( 'NONE',  ( -196.2980642837470100, 20.08915143287812199, -172.1812796682245050 ) ) ;
#6080 = CARTESIAN_POINT ( 'NONE',  ( -122.2593324768321992, 29.00000000000000000, 168.2755348299905052 ) ) ;
#6081 = EDGE_CURVE ( 'NONE', #5508, #2601, #11404, .T. ) ;
#6082 = DIRECTION ( 'NONE',  ( 0.000000000000000000, 0.000000000000000000, -1.000000000000000000 ) ) ;
#6083 = B_SPLINE_CURVE_WITH_KNOTS ( 'NONE', 3,
 ( #12130, #4255, #6200, #3249, #12522, #4187, #3182, #7459, #11532, #8267, #2387, #5185, #5324, #12330, #10254, #10457, #7263, #8335, #11329, #10320, #2191, #7391, #6465, #4318, #9394, #6332, #12393, #5257, #6270 ),
 .UNSPECIFIED., .F., .F.,
 ( 4, 2, 2, 1, 1, 2, 2, 2, 1, 1, 2, 2, 2, 1, 2, 2, 4 ),
 ( 0.000000000000000000, 0.06264877319547468293, 0.09397315979321198276, 0.1096353530920806812, 0.1174664497415151138, 0.1213819980662255715, 0.1252975463909360154, 0.1879463195863035341, 0.2192707061839873350, 0.2349328994828293049, 0.2427639961322546058, 0.2505950927816799068, 0.3132438659770597766, 0.3445682525747496561, 0.3602304458735945958, 0.3758926391724394800, 0.5011901855632154845 ),
 .UNSPECIFIED. ) ;
#6084 = FACE_OUTER_BOUND ( 'NONE', #3132, .T. ) ;
#6085 = DIRECTION ( 'NONE',  ( 0.000000000000000000, 1.000000000000000000, 0.000000000000000000 ) ) ;
#6086 = CARTESIAN_POINT ( 'NONE',  ( 0.000000000000000000, 0.000000000000000000, 0.000000000000000000 ) ) ;
#6087 = CARTESIAN_POINT ( 'NONE',  ( -244.2185274273184064, -8.258776625530128257, 8.357937760093166801 ) ) ;
#6088 = AXIS2_PLACEMENT_3D ( 'NONE', #2698, #9702, #2579 ) ;
#6089 = ORIENTED_EDGE ( 'NONE', *, *, #1874, .T. ) ;
#6090 = CARTESIAN_POINT ( 'NONE',  ( -0.000000000000000000, -22.00000000000000000, 0.000000000000000000 ) ) ;
#6091 = EDGE_CURVE ( 'NONE', #431, #8768, #8655, .T. ) ;
#6092 = CARTESIAN_POINT ( 'NONE',  ( 229.9901544136290568, -2.781634392067636519, 2.136699187716680992 ) ) ;
#6093 = ORIENTED_EDGE ( 'NONE', *, *, #7611, .F. ) ;
#6094 = ORIENTED_EDGE ( 'NONE', *, *, #10701, .T. ) ;
#6095 = DIRECTION ( 'NONE',  ( -0.000000000000000000, 1.000000000000000000, 0.000000000000000000 ) ) ;
#6096 = DIRECTION ( 'NONE',  ( 0.000000000000000000, 1.000000000000000000, 0.000000000000000000 ) ) ;
#6097 = CARTESIAN_POINT ( 'NONE',  ( 172.1812796672219861, 20.08915143311016749, 196.2980642831085163 ) ) ;
#6098 = CARTESIAN_POINT ( 'NONE',  ( -239.3382408973351119, -1.667768204462165116, -11.88390510034685299 ) ) ;
#6099 = DIRECTION ( 'NONE',  ( 0.000000000000000000, 0.5538822189107472926, 0.8325950321581960800 ) ) ;
#6100 = CARTESIAN_POINT ( 'NONE',  ( -245.4266968885101505, 8.952647108375709095, 7.610034337147152605 ) ) ;
#6101 = ORIENTED_EDGE ( 'NONE', *, *, #10363, .T. ) ;
#6102 = CARTESIAN_POINT ( 'NONE',  ( 237.6585102388687289, 20.79694577634646890, 107.6783259591027644 ) ) ;
#6103 = ORIENTED_EDGE ( 'NONE', *, *, #416, .F. ) ;
#6104 = DIRECTION ( 'NONE',  ( 0.000000000000000000, -1.000000000000000000, 0.000000000000000000 ) ) ;
#6105 = EDGE_LOOP ( 'NONE', ( #10960, #2110, #6434, #11286 ) ) ;
#6106 = LINE ( 'NONE', #6045, #673 ) ;
#6107 = CARTESIAN_POINT ( 'NONE',  ( 153.9282213272189495, -30.00000000000000000, 245.7765299597151341 ) ) ;
#6108 = CARTESIAN_POINT ( 'NONE',  ( 161.8917567597108018, 0.000000000000000000, 195.9813743529078920 ) ) ;
#6109 = LINE ( 'NONE', #1039, #10048 ) ;
#6110 = DIRECTION ( 'NONE',  ( 0.000000000000000000, 0.9998057603070480415, -0.01970892327970899874 ) ) ;
#6111 = DIRECTION ( 'NONE',  ( -0.000000000000000000, -1.000000000000000000, 0.000000000000000000 ) ) ;
#6112 = CARTESIAN_POINT ( 'NONE',  ( -130.4544329367273292, 20.79694577634646535, 225.9597979674042563 ) ) ;
#6113 = ORIENTED_EDGE ( 'NONE', *, *, #4231, .F. ) ;
#6114 = CARTESIAN_POINT ( 'NONE',  ( 239.7985776503645354, -1.848645179573700004, 2.971954070984049956 ) ) ;
#6115 = EDGE_LOOP ( 'NONE', ( #3629, #9364, #12642, #221 ) ) ;
#6116 = CARTESIAN_POINT ( 'NONE',  ( -249.4432382447466807, 10.72467464915493984, -4.802290506997906938 ) ) ;
#6117 = FACE_OUTER_BOUND ( 'NONE', #10656, .T. ) ;
#6118 = EDGE_CURVE ( 'NONE', #11136, #5861, #6595, .T. ) ;
#6119 = EDGE_CURVE ( 'NONE', #6702, #1100, #4572, .T. ) ;
#6120 = CARTESIAN_POINT ( 'NONE',  ( -249.6793054724743399, -11.18791971366320404, 3.590677820429848399 ) ) ;
#6121 = VERTEX_POINT ( 'NONE', #2450 ) ;
#6122 = CARTESIAN_POINT ( 'NONE',  ( -259.0935598604229995, 20.79694577620878704, -34.13493237027169158 ) ) ;
#6123 = CARTESIAN_POINT ( 'NONE',  ( -245.8615520219217672, 9.158310437450982278, -7.754087231807664793 ) ) ;
#6124 = CARTESIAN_POINT ( 'NONE',  ( 197.8197553893915028, 18.00000000000000000, -64.27553482998990830 ) ) ;
#6125 = CARTESIAN_POINT ( 'NONE',  ( -244.7823818367005515, -8.610125648031120349, -7.996289175493550339 ) ) ;
#6126 = CIRCLE ( 'NONE', #12508, 250.1999999999999602 ) ;
#6127 =( REPRESENTATION_RELATIONSHIP ('NONE','NONE', #12019, #5191 ) REPRESENTATION_RELATIONSHIP_WITH_TRANSFORMATION ( #12780 )SHAPE_REPRESENTATION_RELATIONSHIP( ) );
#6128 = CARTESIAN_POINT ( 'NONE',  ( -246.0976122680899607, 9.256780778463358672, 7.636466317080543575 ) ) ;
#6129 = PRODUCT_RELATED_PRODUCT_CATEGORY ( 'part', '', ( #439 ) ) ;
#6130 = DIRECTION ( 'NONE',  ( 0.000000000000000000, 0.000000000000000000, 1.000000000000000000 ) ) ;
#6131 = DIRECTION ( 'NONE',  ( 0.7545873610929992870, 0.5538822189107472926, 0.3518698652246467495 ) ) ;
#6132 = CARTESIAN_POINT ( 'NONE',  ( -229.8301233945847457, -7.761986000019901688, 8.855266263419107275 ) ) ;
#6133 = CONTEXT_DEPENDENT_SHAPE_REPRESENTATION ( #426, #1636 ) ;
#6134 = PRODUCT_DEFINITION_SHAPE ( 'NONE', 'NONE',  #13104 ) ;
#6135 = AXIS2_PLACEMENT_3D ( 'NONE', #7361, #9230, #1162 ) ;
#6136 = FACE_OUTER_BOUND ( 'NONE', #9101, .T. ) ;
#6137 = VERTEX_POINT ( 'NONE', #6728 ) ;
#6138 = ORIENTED_EDGE ( 'NONE', *, *, #5661, .F. ) ;
#6139 = CARTESIAN_POINT ( 'NONE',  ( 252.2208631679629889, 20.08915143265645042, -67.55708173926119287 ) ) ;
#6140 = CARTESIAN_POINT ( 'NONE',  ( 149.7885815989021694, -30.00000000000000000, 240.7652044943575333 ) ) ;
#6141 = DIRECTION ( 'NONE',  ( -0.000000000000000000, -1.000000000000000000, 0.000000000000000000 ) ) ;
#6142 = CARTESIAN_POINT ( 'NONE',  ( 197.8197553893920144, 30.00000000000000000, 70.77553482998851564 ) ) ;
#6143 = EDGE_CURVE ( 'NONE', #10691, #4229, #4374, .T. ) ;
#6144 = AXIS2_PLACEMENT_3D ( 'NONE', #420, #4403, #2664 ) ;
#6145 = CARTESIAN_POINT ( 'NONE',  ( 252.4341100441809829, 20.79694577595645910, -67.61424743030308093 ) ) ;
#6146 = AXIS2_PLACEMENT_3D ( 'NONE', #6086, #1010, #2211 ) ;
#6147 = ADVANCED_FACE ( 'NONE', ( #12712 ), #4705, .F. ) ;
#6148 = CARTESIAN_POINT ( 'NONE',  ( -287.1814104624966149, -19.00000000000000000, -23.44910453727290545 ) ) ;
#6149 = DIRECTION ( 'NONE',  ( 0.5735764363510362784, 0.000000000000000000, 0.8191520442889986819 ) ) ;
#6150 = CARTESIAN_POINT ( 'NONE',  ( -244.1927368917095009, -8.241533435392154772, 8.374943118319487567 ) ) ;
#6151 = CONTEXT_DEPENDENT_SHAPE_REPRESENTATION ( #12568, #12595 ) ;
#6152 = ORIENTED_EDGE ( 'NONE', *, *, #7902, .F. ) ;
#6153 = DIRECTION ( 'NONE',  ( 0.000000000000000000, 1.000000000000000000, 0.000000000000000000 ) ) ;
#6154 = DIRECTION ( 'NONE',  ( 1.000000000000000000, 0.000000000000000000, 0.000000000000000000 ) ) ;
#6155 = ORIENTED_EDGE ( 'NONE', *, *, #11761, .F. ) ;
#6156 = ORIENTED_EDGE ( 'NONE', *, *, #12278, .F. ) ;
#6157 = AXIS2_PLACEMENT_3D ( 'NONE', #596, #5727, #5252 ) ;
#6158 = LINE ( 'NONE', #1674, #11250 ) ;
#6159 = DIRECTION ( 'NONE',  ( 0.000000000000000000, 0.000000000000000000, 1.000000000000000000 ) ) ;
#6160 = AXIS2_PLACEMENT_3D ( 'NONE', #4117, #3041, #64 ) ;
#6161 = AXIS2_PLACEMENT_3D ( 'NONE', #2003, #6075, #2328 ) ;
#6162 = CARTESIAN_POINT ( 'NONE',  ( -115.7315435904061331, 19.96883746069636700, -234.7354397749499810 ) ) ;
#6163 = ADVANCED_FACE ( 'NONE', ( #11724 ), #11189, .F. ) ;
#6164 = DIRECTION ( 'NONE',  ( -0.000000000000000000, -1.000000000000000000, 0.000000000000000000 ) ) ;
#6165 = DIRECTION ( 'NONE',  ( 0.9063077870366496036, 0.000000000000000000, 0.4226182617407002740 ) ) ;
#6166 = CARTESIAN_POINT ( 'NONE',  ( -241.5784935620077363, 5.720435375430025893, 10.26436795268994651 ) ) ;
#6167 = PRODUCT_DEFINITION_SHAPE ( 'NONE', 'NONE',  #13094 ) ;
#6168 = AXIS2_PLACEMENT_3D ( 'NONE', #11308, #9104, #910 ) ;
#6169 = VERTEX_POINT ( 'NONE', #7713 ) ;
#6170 = DIRECTION ( 'NONE',  ( 0.4503334343941562956, -0.7071067811865480168, 0.5451603414287978788 ) ) ;
#6171 = EDGE_CURVE ( 'NONE', #12220, #12270, #340, .T. ) ;
#6172 = ORIENTED_EDGE ( 'NONE', *, *, #3080, .F. ) ;
#6173 = CARTESIAN_POINT ( 'NONE',  ( 0.000000000000000000, 22.00000000000000000, -245.7999999999999829 ) ) ;
#6174 = ORIENTED_EDGE ( 'NONE', *, *, #1805, .T. ) ;
#6175 =( REPRESENTATION_RELATIONSHIP ('NONE','NONE', #12019, #182 ) REPRESENTATION_RELATIONSHIP_WITH_TRANSFORMATION ( #378 )SHAPE_REPRESENTATION_RELATIONSHIP( ) );
#6176 = VECTOR ( 'NONE', #208, 1000.000000000000000 ) ;
#6177 = LINE ( 'NONE', #10229, #9189 ) ;
#6178 = CARTESIAN_POINT ( 'NONE',  ( 239.0232640335164263, 0.4900023590031949983, 3.465599286974978543 ) ) ;
#6179 = DIRECTION ( 'NONE',  ( 0.000000000000000000, 1.000000000000000000, 0.000000000000000000 ) ) ;
#6180 = AXIS2_PLACEMENT_3D ( 'NONE', #9570, #6652, #7516 ) ;
#6181 = DIRECTION ( 'NONE',  ( -1.224646799147349509E-16, 0.000000000000000000, -1.000000000000000000 ) ) ;
#6182 = CARTESIAN_POINT ( 'NONE',  ( 71.82423009839129691, 28.60000000000000142, 197.3354503650404865 ) ) ;
#6183 = CARTESIAN_POINT ( 'NONE',  ( -234.0054343868616513, 20.79694577634646535, -115.4021059068222144 ) ) ;
#6184 = CONTEXT_DEPENDENT_SHAPE_REPRESENTATION ( #4124, #5438 ) ;
#6185 = EDGE_LOOP ( 'NONE', ( #7023, #10897, #7752, #6824 ) ) ;
#6186 = DIRECTION ( 'NONE',  ( 0.000000000000000000, -1.000000000000000000, 0.000000000000000000 ) ) ;
#6187 = ORIENTED_EDGE ( 'NONE', *, *, #9123, .T. ) ;
#6188 = CARTESIAN_POINT ( 'NONE',  ( 224.4939760857161843, 6.051844909775672576, -0.1192985195352703198 ) ) ;
#6189 = CARTESIAN_POINT ( 'NONE',  ( -247.6855308000310743, -9.751870871334467950, -6.992977238237519266 ) ) ;
#6190 = AXIS2_PLACEMENT_3D ( 'NONE', #3327, #12726, #1537 ) ;
#6191 = FACE_OUTER_BOUND ( 'NONE', #5088, .T. ) ;
#6192 = ORIENTED_EDGE ( 'NONE', *, *, #4259, .F. ) ;
#6193 = CARTESIAN_POINT ( 'NONE',  ( 172.3268284089184874, 20.79694577645659948, 196.4640694358555209 ) ) ;
#6194 = CARTESIAN_POINT ( 'NONE',  ( -243.0412680634588583, 7.360923497056134579, -9.480357583680490308 ) ) ;
#6195 = DIRECTION ( 'NONE',  ( -0.000000000000000000, -1.000000000000000000, 0.000000000000000000 ) ) ;
#6196 = VECTOR ( 'NONE', #2048, 1000.000000000000114 ) ;
#6197 = CARTESIAN_POINT ( 'NONE',  ( -243.1833766790699087, -7.470616520369461888, -9.069320236344923458 ) ) ;
#6198 = EDGE_CURVE ( 'NONE', #1725, #8820, #1187, .T. ) ;
#6199 = EDGE_LOOP ( 'NONE', ( #5069, #9711, #8824, #5295 ) ) ;
#6200 = CARTESIAN_POINT ( 'NONE',  ( 239.6582758811249789, -1.713542963182288936, 3.052483991793907947 ) ) ;
#6201 = DIRECTION ( 'NONE',  ( -0.1736481776669207000, 0.000000000000000000, -0.9848077530122097967 ) ) ;
#6202 = LINE ( 'NONE', #394, #530 ) ;
#6203 = CARTESIAN_POINT ( 'NONE',  ( 197.8197553893920144, 30.00000000000000000, 64.27553482998850143 ) ) ;
#6204 = ORIENTED_EDGE ( 'NONE', *, *, #11419, .T. ) ;
#6205 = EDGE_LOOP ( 'NONE', ( #3684, #2611, #11370, #661 ) ) ;
#6206 = AXIS2_PLACEMENT_3D ( 'NONE', #11653, #3710, #2572 ) ;
#6207 =( REPRESENTATION_RELATIONSHIP ('NONE','NONE', #12019, #5191 ) REPRESENTATION_RELATIONSHIP_WITH_TRANSFORMATION ( #12134 )SHAPE_REPRESENTATION_RELATIONSHIP( ) );
#6208 = CARTESIAN_POINT ( 'NONE',  ( -247.2466869553009872, 20.08915143298854389, 83.95474316008009907 ) ) ;
#6209 = LINE ( 'NONE', #3123, #5502 ) ;
#6210 = CARTESIAN_POINT ( 'NONE',  ( 239.2334266249513917, -1.105838440500075848, -3.321566349845947119 ) ) ;
#6211 = CARTESIAN_POINT ( 'NONE',  ( 233.5975020798683204, 0.000000000000000000, 0.000000000000000000 ) ) ;
#6212 = DIRECTION ( 'NONE',  ( -0.000000000000000000, -1.000000000000000000, 0.000000000000000000 ) ) ;
#6213 = EDGE_CURVE ( 'NONE', #157, #3155, #1392, .T. ) ;
#6214 = AXIS2_PLACEMENT_3D ( 'NONE', #1710, #11907, #5707 ) ;
#6215 = CARTESIAN_POINT ( 'NONE',  ( 71.82423009839129691, 30.00000000000000000, -197.3354503650404865 ) ) ;
#6216 = CARTESIAN_POINT ( 'NONE',  ( 0.000000000000000000, 0.000000000000000000, 0.000000000000000000 ) ) ;
#6217 = CARTESIAN_POINT ( 'NONE',  ( -241.3472527821318181, -5.384021912605467364, 10.44389002220115614 ) ) ;
#6218 = CONTEXT_DEPENDENT_SHAPE_REPRESENTATION ( #487, #12088 ) ;
#6219 = ITEM_DEFINED_TRANSFORMATION ( 'NONE', 'NONE', #399,  #805 ) ;
#6220 = ORIENTED_EDGE ( 'NONE', *, *, #12321, .F. ) ;
#6221 = AXIS2_PLACEMENT_3D ( 'NONE', #12306, #7245, #2371 ) ;
#6222 = CARTESIAN_POINT ( 'NONE',  ( -294.1869546181095529, -19.00000000000000000, -31.92980917095500359 ) ) ;
#6223 = CARTESIAN_POINT ( 'NONE',  ( 229.9760382323824501, -1.128309064994147626, 3.321078061868915743 ) ) ;
#6224 = ORIENTED_EDGE ( 'NONE', *, *, #4183, .T. ) ;
#6225 = ORIENTED_EDGE ( 'NONE', *, *, #464, .T. ) ;
#6226 = EDGE_CURVE ( 'NONE', #1949, #11299, #7064, .T. ) ;
#6227 = EDGE_CURVE ( 'NONE', #4886, #12985, #7542, .T. ) ;
#6228 = CYLINDRICAL_SURFACE ( 'NONE', #9348, 3.000000000000000000 ) ;
#6229 = DIRECTION ( 'NONE',  ( 0.000000000000000000, 0.000000000000000000, -1.000000000000000000 ) ) ;
#6230 = VECTOR ( 'NONE', #10004, 1000.000000000000000 ) ;
#6231 = CONICAL_SURFACE ( 'NONE', #2595, 6.500000000000000888, 0.7853981633974617127 ) ;
#6232 = CARTESIAN_POINT ( 'NONE',  ( -226.6392846536229229, 19.96883746130017911, -130.8783844628770794 ) ) ;
#6233 = CARTESIAN_POINT ( 'NONE',  ( -239.4988366478256125, -1.826140896386560186, -11.86023454918143472 ) ) ;
#6234 = DIRECTION ( 'NONE',  ( 1.000000000000000000, 0.000000000000000000, 0.000000000000000000 ) ) ;
#6235 = VECTOR ( 'NONE', #4071, 1000.000000000000000 ) ;
#6236 = CARTESIAN_POINT ( 'NONE',  ( -241.3731105455106842, 5.422910281599071958, 10.42375653614991826 ) ) ;
#6237 = EDGE_LOOP ( 'NONE', ( #4085, #289 ) ) ;
#6238 = DIRECTION ( 'NONE',  ( 0.000000000000000000, 0.9998057603070481525, -0.01970892327970900221 ) ) ;
#6239 = EDGE_LOOP ( 'NONE', ( #10741, #853, #5972 ) ) ;
#6240 = DIRECTION ( 'NONE',  ( 1.000000000000000000, 0.000000000000000000, 0.000000000000000000 ) ) ;
#6241 = EDGE_LOOP ( 'NONE', ( #984, #890, #4401, #3334 ) ) ;
#6242 = ORIENTED_EDGE ( 'NONE', *, *, #1586, .F. ) ;
#6243 = EDGE_CURVE ( 'NONE', #8825, #3483, #2436, .T. ) ;
#6244 = ADVANCED_FACE ( 'NONE', ( #11495 ), #9177, .F. ) ;
#6245 = VECTOR ( 'NONE', #11710, 1000.000000000000114 ) ;
#6246 = CARTESIAN_POINT ( 'NONE',  ( -0.000000000000000000, -25.00000000000000000, 0.000000000000000000 ) ) ;
#6247 = CARTESIAN_POINT ( 'NONE',  ( 239.4370728336666048, 1.442813601903317977, 3.188799201111035320 ) ) ;
#6248 = CARTESIAN_POINT ( 'NONE',  ( 0.000000000000000000, -2.957522019940860139E-14, 0.000000000000000000 ) ) ;
#6249 = EDGE_CURVE ( 'NONE', #1505, #1172, #4109, .T. ) ;
#6250 = CARTESIAN_POINT ( 'NONE',  ( -130.3442252640560923, 20.08915143297736705, -225.7689075324038299 ) ) ;
#6251 = CARTESIAN_POINT ( 'NONE',  ( -122.2593324768359935, 29.00000000000000000, -168.2755348299880040 ) ) ;
#6252 = CIRCLE ( 'NONE', #503, 12.00000000000000000 ) ;
#6253 = AXIS2_PLACEMENT_3D ( 'NONE', #7565, #8444, #11639 ) ;
#6254 = AXIS2_PLACEMENT_3D ( 'NONE', #9180, #7249, #9251 ) ;
#6255 = ORIENTED_EDGE ( 'NONE', *, *, #12085, .F. ) ;
#6256 = AXIS2_PLACEMENT_3D ( 'NONE', #2462, #6409, #5464 ) ;
#6257 = CLOSED_SHELL ( 'NONE', ( #5659, #4718, #9321, #2862, #12107, #8761, #818, #7824, #5903, #9463, #777, #12332, #8669, #9688, #5078, #5905, #9949, #10865, #13, #1844, #1343, #12492, #8767, #9573, #10643, #6632, #7339, #176, #9232, #3030, #12962, #10264, #10528, #11706, #10053, #9415, #4993, #5408, #4720, #11081, #8448, #10887, #297, #8158, #8292, #923, #8364, #4108, #5883, #5884, #2644, #3847, #578, #8012, #3262, #9565, #1103, #4116, #939, #460, #12817, #10216, #4521, #7588, #9295, #12439, #11428, #8512, #9765, #1915, #8843, #10435, #5301, #4820, #2150, #6034, #7455, #5080, #11599, #2007, #754, #12944, #12494, #11946, #6364, #12365, #13008, #9296, #10029, #6391, #3055, #10786, #7757, #4745, #12198, #8260, #1964, #9093, #1588, #10594, #8721, #10788, #10837, #2062, #7853, #3219, #682, #12819, #9076, #4639, #4748, #10561, #10932, #6074, #8811, #6571, #8028, #7823, #6331, #2443, #8486, #137, #3702, #7809, #9335, #2389, #1629, #12591, #10462, #11849, #3294, #8076, #602, #7274, #3672 ) ) ;
#6258 = CARTESIAN_POINT ( 'NONE',  ( -197.8197553893909912, 30.00000000000000000, 69.77553482999131518 ) ) ;
#6259 = ORIENTED_EDGE ( 'NONE', *, *, #10275, .T. ) ;
#6260 = CIRCLE ( 'NONE', #9645, 239.8169934640465044 ) ;
#6261 = DIRECTION ( 'NONE',  ( -0.000000000000000000, -1.000000000000000000, 0.000000000000000000 ) ) ;
#6262 = CARTESIAN_POINT ( 'NONE',  ( -247.2298618823421066, -9.638957510065514711, -7.147826786427922130 ) ) ;
#6263 = CARTESIAN_POINT ( 'NONE',  ( -248.5980333526342179, -9.980365686173904294, 6.207212898096353015 ) ) ;
#6264 = ORIENTED_EDGE ( 'NONE', *, *, #10718, .T. ) ;
#6265 = VECTOR ( 'NONE', #11366, 1000.000000000000000 ) ;
#6266 = CARTESIAN_POINT ( 'NONE',  ( 247.4557548098379982, 20.79694577642534270, 84.02568524150230189 ) ) ;
#6267 = CARTESIAN_POINT ( 'NONE',  ( -244.8216528713956563, 8.638952368661110270, -8.328775923151233940 ) ) ;
#6268 = CARTESIAN_POINT ( 'NONE',  ( 287.1814104624967854, -29.00000000000000000, 23.44910453727084132 ) ) ;
#6269 = CARTESIAN_POINT ( 'NONE',  ( -245.2557111518780459, -8.868800241211268087, -7.708496933118081706 ) ) ;
#6270 = CARTESIAN_POINT ( 'NONE',  ( 238.9743710777160857, 8.519355453646930632E-11, 3.499999942258626984 ) ) ;
#6271 = DIRECTION ( 'NONE',  ( 0.3420201433256790380, 0.000000000000000000, -0.9396926207859046531 ) ) ;
#6272 = CARTESIAN_POINT ( 'NONE',  ( 240.5378997430644858, 3.246179723024485764, 1.312253685488862009 ) ) ;
#6273 = AXIS2_PLACEMENT_3D ( 'NONE', #1314, #2966, #5239 ) ;
#6274 = CONTEXT_DEPENDENT_SHAPE_REPRESENTATION ( #7658, #9953 ) ;
#6275 = PLANE ( 'NONE',  #4506 ) ;
#6276 = EDGE_LOOP ( 'NONE', ( #1173, #749, #143, #4118 ) ) ;
#6277 = CARTESIAN_POINT ( 'NONE',  ( 158.9353507248500250, 20.08915143321791419, 207.1687172302519855 ) ) ;
#6278 = CARTESIAN_POINT ( 'NONE',  ( 0.000000000000000000, -20.00000000000000000, 0.000000000000000000 ) ) ;
#6279 = CARTESIAN_POINT ( 'NONE',  ( -248.7692280201405310, 10.08940167824826339, 6.022204372445879805 ) ) ;
#6280 = VECTOR ( 'NONE', #10894, 1000.000000000000000 ) ;
#6281 = FACE_BOUND ( 'NONE', #8725, .T. ) ;
#6282 = CIRCLE ( 'NONE', #12874, 304.0000000000000000 ) ;
#6283 = CARTESIAN_POINT ( 'NONE',  ( 71.82423009839129691, 19.40000000000000213, 202.4354503650404808 ) ) ;
#6284 = CARTESIAN_POINT ( 'NONE',  ( -248.0636855464110795, -9.829232304199436498, 6.883789224096078740 ) ) ;
#6285 = FACE_OUTER_BOUND ( 'NONE', #7119, .T. ) ;
#6286 = DIRECTION ( 'NONE',  ( 0.9961946980917455452, 0.000000000000000000, 0.08715574274765836016 ) ) ;
#6287 = DIRECTION ( 'NONE',  ( 0.000000000000000000, 1.000000000000000000, 0.000000000000000000 ) ) ;
#6288 = ORIENTED_EDGE ( 'NONE', *, *, #12515, .F. ) ;
#6289 = DIRECTION ( 'NONE',  ( 0.000000000000000000, 1.000000000000000000, 0.000000000000000000 ) ) ;
#6290 =( GEOMETRIC_REPRESENTATION_CONTEXT ( 3 ) GLOBAL_UNCERTAINTY_ASSIGNED_CONTEXT ( ( #919 ) ) GLOBAL_UNIT_ASSIGNED_CONTEXT ( ( #5049, #9327, #2257 ) ) REPRESENTATION_CONTEXT ( 'NONE', 'WORKASPACE' ) );
#6291 = PRODUCT_DEFINITION_SHAPE ( 'NONE', 'NONE',  #13055 ) ;
#6292 = DIRECTION ( 'NONE',  ( 0.000000000000000000, 0.000000000000000000, 1.000000000000000000 ) ) ;
#6293 = VERTEX_POINT ( 'NONE', #12248 ) ;
#6294 = EDGE_CURVE ( 'NONE', #320, #10564, #2459, .T. ) ;
#6295 = VERTEX_POINT ( 'NONE', #12554 ) ;
#6296 = ADVANCED_FACE ( 'NONE', ( #11237 ), #9062, .F. ) ;
#6297 = CYLINDRICAL_SURFACE ( 'NONE', #9117, 5.499999999999986677 ) ;
#6298 = FACE_OUTER_BOUND ( 'NONE', #2271, .T. ) ;
#6299 = CARTESIAN_POINT ( 'NONE',  ( 159.3024069661366866, 19.96883746137792670, -207.6469600131167681 ) ) ;
#6300 = DIRECTION ( 'NONE',  ( 0.000000000000000000, 0.000000000000000000, 1.000000000000000000 ) ) ;
#6301 = DIRECTION ( 'NONE',  ( -0.6427876096865405842, 0.000000000000000000, 0.7660444431189772363 ) ) ;
#6302 = VECTOR ( 'NONE', #3154, 1000.000000000000114 ) ;
#6303 = CARTESIAN_POINT ( 'NONE',  ( -242.5648157350879899, 6.889953638923882906, 9.518299937401890176 ) ) ;
#6304 = ORIENTED_EDGE ( 'NONE', *, *, #4083, .T. ) ;
#6305 = CARTESIAN_POINT ( 'NONE',  ( 151.9741924115233189, 20.79694577634646180, 212.0849693193238181 ) ) ;
#6306 = ORIENTED_EDGE ( 'NONE', *, *, #3516, .T. ) ;
#6307 = CARTESIAN_POINT ( 'NONE',  ( 0.000000000000000000, -20.00000000000000000, 0.000000000000000000 ) ) ;
#6308 = VERTEX_POINT ( 'NONE', #4476 ) ;
#6309 = ORIENTED_EDGE ( 'NONE', *, *, #6858, .T. ) ;
#6310 = AXIS2_PLACEMENT_3D ( 'NONE', #9081, #8017, #12076 ) ;
#6311 =( REPRESENTATION_RELATIONSHIP ('NONE','NONE', #12019, #5191 ) REPRESENTATION_RELATIONSHIP_WITH_TRANSFORMATION ( #5458 )SHAPE_REPRESENTATION_RELATIONSHIP( ) );
#6312 = FACE_OUTER_BOUND ( 'NONE', #3902, .T. ) ;
#6313 = CARTESIAN_POINT ( 'NONE',  ( -250.0000000000000000, 1.000000000000000000, -11.95826074310140008 ) ) ;
#6314 = CARTESIAN_POINT ( 'NONE',  ( 235.4000000000000057, -2.999417280921144346, 0.05912676983912699968 ) ) ;
#6315 = CARTESIAN_POINT ( 'NONE',  ( 239.4975972760159948, 1.524294660007503355, -3.150668453783941114 ) ) ;
#6316 = CARTESIAN_POINT ( 'NONE',  ( -238.7193995381545335, 0.2079802334036294775, -11.74814885867293413 ) ) ;
#6317 = DIRECTION ( 'NONE',  ( 0.6368676505102707219, 0.000000000000000000, 0.7709731485165535192 ) ) ;
#6318 = ADVANCED_FACE ( 'NONE', ( #3482 ), #3944, .T. ) ;
#6319 = EDGE_CURVE ( 'NONE', #1045, #7994, #5445, .T. ) ;
#6320 = ORIENTED_EDGE ( 'NONE', *, *, #10030, .T. ) ;
#6321 = CARTESIAN_POINT ( 'NONE',  ( -0.000000000000000000, -3.061616997868385015E-14, 0.000000000000000000 ) ) ;
#6322 = EDGE_LOOP ( 'NONE', ( #2551, #6417 ) ) ;
#6323 = CARTESIAN_POINT ( 'NONE',  ( -122.2593324768321992, 29.00000000000000000, 173.7755348299905052 ) ) ;
#6324 = CARTESIAN_POINT ( 'NONE',  ( -246.9756885463878859, -9.564884954983938314, -7.246373649491316016 ) ) ;
#6325 = CARTESIAN_POINT ( 'NONE',  ( -197.8197553893909912, 19.00000000000000000, 64.27553482999130097 ) ) ;
#6326 = ORIENTED_EDGE ( 'NONE', *, *, #3506, .F. ) ;
#6327 = CARTESIAN_POINT ( 'NONE',  ( 259.0935598591524922, 20.79694577673652134, -34.13493237036694694 ) ) ;
#6328 = CARTESIAN_POINT ( 'NONE',  ( -244.1910629329458970, 8.248580893023101268, -8.715491049894939835 ) ) ;
#6329 = CARTESIAN_POINT ( 'NONE',  ( -238.9284634072548670, 1.043171514628518537, 11.95464273948973322 ) ) ;
#6330 = CARTESIAN_POINT ( 'NONE',  ( -242.0448478369141299, -6.321212806544949991, -9.907269457473429242 ) ) ;
#6331 = ADVANCED_FACE ( 'NONE', ( #11759 ), #972, .F. ) ;
#6332 = CARTESIAN_POINT ( 'NONE',  ( 239.0381261355857703, -0.5585874493611364677, 3.455211367194953809 ) ) ;
#6333 = PRODUCT_CONTEXT ( 'NONE', #13001, 'mechanical' ) ;
#6334 = CARTESIAN_POINT ( 'NONE',  ( 240.4535390813594233, 3.009067775009412582, -1.828999331050441102 ) ) ;
#6335 = CONTEXT_DEPENDENT_SHAPE_REPRESENTATION ( #5184, #360 ) ;
#6336 = FACE_OUTER_BOUND ( 'NONE', #1831, .T. ) ;
#6337 = ORIENTED_EDGE ( 'NONE', *, *, #2863, .T. ) ;
#6338 = TOROIDAL_SURFACE ( 'NONE', #585, 241.5000000000000000, 2.500000000000000000 ) ;
#6339 = CARTESIAN_POINT ( 'NONE',  ( -252.2208631657525473, 20.08915143310922957, 67.55708173876999467 ) ) ;
#6340 = CYLINDRICAL_SURFACE ( 'NONE', #311, 249.7999999999999829 ) ;
#6341 = LINE ( 'NONE', #10393, #9973 ) ;
#6342 = CARTESIAN_POINT ( 'NONE',  ( 239.6467530156110683, -1.711397834369177140, -3.057326064312821945 ) ) ;
#6343 = DIRECTION ( 'NONE',  ( 0.000000000000000000, -1.000000000000000000, 0.000000000000000000 ) ) ;
#6344 = ADVANCED_BREP_SHAPE_REPRESENTATION ( '', ( #10352, #805 ), #2501 ) ;
#6345 = CARTESIAN_POINT ( 'NONE',  ( -246.8633775110742476, -9.531357831541830805, 7.291317142722177458 ) ) ;
#6346 = DIRECTION ( 'NONE',  ( -0.7709731485165536302, 0.000000000000000000, 0.6368676505102706109 ) ) ;
#6347 = DIRECTION ( 'NONE',  ( 0.7071067811865463515, 0.000000000000000000, 0.7071067811865487940 ) ) ;
#6348 = DIRECTION ( 'NONE',  ( 0.000000000000000000, -1.000000000000000000, 0.000000000000000000 ) ) ;
#6349 = AXIS2_PLACEMENT_3D ( 'NONE', #1423, #6694, #11561 ) ;
#6350 = EDGE_LOOP ( 'NONE', ( #8760, #9919, #11538, #12464 ) ) ;
#6351 = DIRECTION ( 'NONE',  ( 0.000000000000000000, 0.000000000000000000, -1.000000000000000000 ) ) ;
#6352 = CARTESIAN_POINT ( 'NONE',  ( 229.9785025033683326, -1.551323116862773244, -3.145807476139447889 ) ) ;
#6353 = EDGE_LOOP ( 'NONE', ( #2766, #11268, #12575, #9811 ) ) ;
#6354 = VERTEX_POINT ( 'NONE', #10749 ) ;
#6355 = CARTESIAN_POINT ( 'NONE',  ( 225.1241593668336236, -29.00000000000000000, -185.9653539489990521 ) ) ;
#6356 = DIRECTION ( 'NONE',  ( 0.000000000000000000, 1.000000000000000000, 0.000000000000000000 ) ) ;
#6357 = CIRCLE ( 'NONE', #12951, 5.500000000000015099 ) ;
#6358 = AXIS2_PLACEMENT_3D ( 'NONE', #3480, #3610, #7678 ) ;
#6359 = B_SPLINE_CURVE_WITH_KNOTS ( 'NONE', 3,
 ( #6068, #12197, #12128, #1867, #11125, #10123, #11191, #10465, #11643, #2498, #3695, #11774, #11512 ),
 .UNSPECIFIED., .F., .F.,
 ( 4, 2, 2, 1, 2, 2, 4 ),
 ( 0.000000000000000000, 0.2500000000000000000, 0.4999999999999999445, 0.6250000000000000000, 0.6875000000000000000, 0.7500000000000000000, 1.000000000000000000 ),
 .UNSPECIFIED. ) ;
#6360 = CARTESIAN_POINT ( 'NONE',  ( -115.8123742918135832, 20.55460285136280518, 234.8993005745464586 ) ) ;
#6361 = DIRECTION ( 'NONE',  ( 0.6368676505102709440, 0.000000000000000000, 0.7709731485165532971 ) ) ;
#6362 = DIRECTION ( 'NONE',  ( 0.000000000000000000, 0.000000000000000000, 1.000000000000000000 ) ) ;
#6363 = CARTESIAN_POINT ( 'NONE',  ( 0.000000000000000000, 30.00000000000000000, -201.4999999999999716 ) ) ;
#6364 = ADVANCED_FACE ( 'NONE', ( #7879 ), #8850, .F. ) ;
#6365 = ADVANCED_FACE ( 'NONE', ( #1619 ), #11882, .F. ) ;
#6366 = EDGE_LOOP ( 'NONE', ( #4360, #3779, #6945, #12965 ) ) ;
#6367 = AXIS2_PLACEMENT_3D ( 'NONE', #10373, #1247, #250 ) ;
#6368 = CARTESIAN_POINT ( 'NONE',  ( 224.4939760857161843, 0.000000000000000000, 0.000000000000000000 ) ) ;
#6370 = ORIENTED_EDGE ( 'NONE', *, *, #512, .F. ) ;
#6369 = AXIS2_PLACEMENT_3D ( 'NONE', #4786, #5663, #3923 ) ;
#6371 = VECTOR ( 'NONE', #435, 1000.000000000000000 ) ;
#6372 = DIRECTION ( 'NONE',  ( 0.000000000000000000, 0.9998057603070480415, -0.01970892327970899527 ) ) ;
#6373 = ORIENTED_EDGE ( 'NONE', *, *, #10460, .F. ) ;
#6374 = ORIENTED_EDGE ( 'NONE', *, *, #3862, .F. ) ;
#6375 = CONICAL_SURFACE ( 'NONE', #5422, 5.499999999999986677, 0.7853981633974461696 ) ;
#6376 = AXIS2_PLACEMENT_3D ( 'NONE', #2522, #4387, #3383 ) ;
#6377 = DIRECTION ( 'NONE',  ( 0.000000000000000000, 1.000000000000000000, 0.000000000000000000 ) ) ;
#6378 = DIRECTION ( 'NONE',  ( 1.000000000000000000, 0.000000000000000000, 0.000000000000000000 ) ) ;
#6379 = CARTESIAN_POINT ( 'NONE',  ( 239.2304539311643623, 1.097329040102013931, -3.323615143739755862 ) ) ;
#6380 = DIRECTION ( 'NONE',  ( -0.000000000000000000, -1.000000000000000000, 0.000000000000000000 ) ) ;
#6381 = CARTESIAN_POINT ( 'NONE',  ( -243.2722961588427495, 7.557668642214872889, 9.321309795288598821 ) ) ;
#6382 =( GEOMETRIC_REPRESENTATION_CONTEXT ( 3 ) GLOBAL_UNCERTAINTY_ASSIGNED_CONTEXT ( ( #3973 ) ) GLOBAL_UNIT_ASSIGNED_CONTEXT ( ( #8905, #7243, #11307 ) ) REPRESENTATION_CONTEXT ( 'NONE', 'WORKASPACE' ) );
#6383 = ORIENTED_EDGE ( 'NONE', *, *, #1030, .F. ) ;
#6384 = CARTESIAN_POINT ( 'NONE',  ( -122.2593324768359935, 19.00000000000000000, -162.7755348299880040 ) ) ;
#6385 = ORIENTED_EDGE ( 'NONE', *, *, #8882, .F. ) ;
#6386 = LINE ( 'NONE', #12313, #7835 ) ;
#6387 = DIRECTION ( 'NONE',  ( 1.000000000000000000, 0.000000000000000000, 0.000000000000000000 ) ) ;
#6388 = AXIS2_PLACEMENT_3D ( 'NONE', #10631, #1499, #10504 ) ;
#6389 = CARTESIAN_POINT ( 'NONE',  ( 258.4638482596385529, 20.08915143297736705, -34.02434144668546168 ) ) ;
#6390 = ORIENTED_EDGE ( 'NONE', *, *, #7901, .T. ) ;
#6391 = ADVANCED_FACE ( 'NONE', ( #4606 ), #2035, .F. ) ;
#6392 = AXIS2_PLACEMENT_3D ( 'NONE', #2506, #12516, #11652 ) ;
#6393 = DIRECTION ( 'NONE',  ( 0.000000000000000000, 1.000000000000000000, 0.000000000000000000 ) ) ;
#6394 = EDGE_CURVE ( 'NONE', #7801, #4948, #7778, .T. ) ;
#6395 = CARTESIAN_POINT ( 'NONE',  ( -242.3889174921309291, 6.718220501240577569, -9.943174754796373804 ) ) ;
#6396 = CARTESIAN_POINT ( 'NONE',  ( 185.9653539490014111, -19.00000000000000000, 225.1241593668316625 ) ) ;
#6397 = DIRECTION ( 'NONE',  ( -0.000000000000000000, -1.000000000000000000, 0.000000000000000000 ) ) ;
#6398 = AXIS2_PLACEMENT_3D ( 'NONE', #2527, #4520, #4455 ) ;
#6399 = PRODUCT ( 'Drain Plug', 'Drain Plug', '', ( #6333 ) ) ;
#6400 = PRODUCT_CONTEXT ( 'NONE', #9515, 'mechanical' ) ;
#6401 = CARTESIAN_POINT ( 'NONE',  ( -229.6905319492641979, 1.370232268880117621, -11.92730036543203909 ) ) ;
#6402 = CONTEXT_DEPENDENT_SHAPE_REPRESENTATION ( #7407, #575 ) ;
#6403 = AXIS2_PLACEMENT_3D ( 'NONE', #12267, #2058, #1201 ) ;
#6404 = DIRECTION ( 'NONE',  ( -0.6368676505102689456, 0.000000000000000000, -0.7709731485165549625 ) ) ;
#6405 = ORIENTED_EDGE ( 'NONE', *, *, #11171, .F. ) ;
#6406 = CARTESIAN_POINT ( 'NONE',  ( 207.6469600143036587, 19.96883745899249618, -159.3024069668460072 ) ) ;
#6407 = EDGE_CURVE ( 'NONE', #10097, #11992, #11825, .T. ) ;
#6408 = DIRECTION ( 'NONE',  ( 0.000000000000000000, 0.000000000000000000, -1.000000000000000000 ) ) ;
#6409 = DIRECTION ( 'NONE',  ( -0.000000000000000000, -1.000000000000000000, 0.000000000000000000 ) ) ;
#6410 = DIRECTION ( 'NONE',  ( -0.000000000000000000, 0.01970892327970912364, 0.9998057603070482635 ) ) ;
#6411 = CARTESIAN_POINT ( 'NONE',  ( -8.533827019709523398, 20.79694577634646180, -260.7745447061711843 ) ) ;
#6412 = CARTESIAN_POINT ( 'NONE',  ( 0.000000000000000000, 21.50000000000000000, 0.000000000000000000 ) ) ;
#6413 = ADVANCED_FACE ( 'NONE', ( #10683 ), #7152, .F. ) ;
#6414 = DIRECTION ( 'NONE',  ( 0.5363228529974877201, -0.1961161351381840168, -0.8209118459926720845 ) ) ;
#6415 = CARTESIAN_POINT ( 'NONE',  ( -41.21542755584192008, -138.4705547276867321, -7.267391899530232457 ) ) ;
#6416 = CARTESIAN_POINT ( 'NONE',  ( -246.6344430662078366, -9.451372532214236344, 6.980988236095548416 ) ) ;
#6417 = ORIENTED_EDGE ( 'NONE', *, *, #4600, .F. ) ;
#6418 = CYLINDRICAL_SURFACE ( 'NONE', #5329, 5.500000000000005329 ) ;
#6419 = CARTESIAN_POINT ( 'NONE',  ( -240.5118714936808999, -3.871746541839889755, 11.35824976270681574 ) ) ;
#6420 = DIRECTION ( 'NONE',  ( 0.000000000000000000, 0.000000000000000000, 1.000000000000000000 ) ) ;
#6421 = VERTEX_POINT ( 'NONE', #4808 ) ;
#6422 = ORIENTED_EDGE ( 'NONE', *, *, #7578, .F. ) ;
#6423 = DIRECTION ( 'NONE',  ( 0.000000000000000000, 0.9998057603070481525, -0.01970892327970899874 ) ) ;
#6424 = FACE_OUTER_BOUND ( 'NONE', #5417, .T. ) ;
#6425 = CIRCLE ( 'NONE', #8554, 239.0000000000000000 ) ;
#6426 = CARTESIAN_POINT ( 'NONE',  ( -259.6535381484769118, 20.55460285079236016, -34.20858920326526942 ) ) ;
#6427 = CARTESIAN_POINT ( 'NONE',  ( -107.5873595010537684, 20.08915143297736705, -237.4577367525705824 ) ) ;
#6428 = DIRECTION ( 'NONE',  ( -0.000000000000000000, -1.000000000000000000, 0.000000000000000000 ) ) ;
#6429 =( REPRESENTATION_RELATIONSHIP ('NONE','NONE', #12019, #182 ) REPRESENTATION_RELATIONSHIP_WITH_TRANSFORMATION ( #11238 )SHAPE_REPRESENTATION_RELATIONSHIP( ) );
#6430 = PRODUCT_DEFINITION_SHAPE ( 'NONE', 'NONE',  #13177 ) ;
#6431 = DIRECTION ( 'NONE',  ( -0.9848077530122085754, 0.000000000000000000, 0.1736481776669273613 ) ) ;
#6432 = LINE ( 'NONE', #1361, #7316 ) ;
#6433 = CARTESIAN_POINT ( 'NONE',  ( -254.0989678903617914, 20.79694577634646535, -59.24444182677505211 ) ) ;
#6434 = ORIENTED_EDGE ( 'NONE', *, *, #4038, .F. ) ;
#6435 = CARTESIAN_POINT ( 'NONE',  ( 212.0849693193239318, 20.79694577634646180, -151.9741924115230347 ) ) ;
#6436 = EDGE_LOOP ( 'NONE', ( #2700, #245, #873, #6617 ) ) ;
#6437 = DIRECTION ( 'NONE',  ( 0.000000000000000000, 1.000000000000000000, 0.000000000000000000 ) ) ;
#6438 = ORIENTED_EDGE ( 'NONE', *, *, #8205, .T. ) ;
#6439 = EDGE_LOOP ( 'NONE', ( #10211, #3818, #2704, #9302, #5024, #9762 ) ) ;
#6440 = CONICAL_SURFACE ( 'NONE', #6221, 6.500000000000005329, 0.7853981633974547183 ) ;
#6441 = EDGE_CURVE ( 'NONE', #1401, #368, #3734, .T. ) ;
#6442 = CARTESIAN_POINT ( 'NONE',  ( 227.3999999999999773, 4.499125921381716076, -0.08869015475868961829 ) ) ;
#6443 = DIRECTION ( 'NONE',  ( -0.000000000000000000, -1.000000000000000000, 0.000000000000000000 ) ) ;
#6444 = CARTESIAN_POINT ( 'NONE',  ( 0.000000000000000000, 9.797174393178825657E-16, 242.0000000000000000 ) ) ;
#6445 = CARTESIAN_POINT ( 'NONE',  ( 7.960204194457795477E-16, 30.00000000000000000, -214.5000000000000000 ) ) ;
#6446 = DIRECTION ( 'NONE',  ( 0.7709731485165535192, -0.000000000000000000, -0.6368676505102707219 ) ) ;
#6447 = CIRCLE ( 'NONE', #3018, 5.100000000000017408 ) ;
#6448 = VERTEX_POINT ( 'NONE', #3745 ) ;
#6449 = DIRECTION ( 'NONE',  ( 0.000000000000000000, 1.000000000000000000, 0.000000000000000000 ) ) ;
#6450 = AXIS2_PLACEMENT_3D ( 'NONE', #6623, #3809, #558 ) ;
#6451 = ORIENTED_EDGE ( 'NONE', *, *, #2540, .F. ) ;
#6452 =( GEOMETRIC_REPRESENTATION_CONTEXT ( 3 ) GLOBAL_UNCERTAINTY_ASSIGNED_CONTEXT ( ( #9983 ) ) GLOBAL_UNIT_ASSIGNED_CONTEXT ( ( #10967, #3626, #1898 ) ) REPRESENTATION_CONTEXT ( 'NONE', 'WORKASPACE' ) );
#6453 = DIRECTION ( 'NONE',  ( -0.000000000000000000, -1.000000000000000000, 0.000000000000000000 ) ) ;
#6454 = CARTESIAN_POINT ( 'NONE',  ( -210.0000000000000000, 30.00000000000000000, -6.500000000000000000 ) ) ;
#6455 = CARTESIAN_POINT ( 'NONE',  ( 237.4577367525706109, 20.08915143297736705, -107.5873595010537542 ) ) ;
#6456 = ORIENTED_EDGE ( 'NONE', *, *, #9388, .T. ) ;
#6457 = EDGE_CURVE ( 'NONE', #10014, #11841, #5459, .T. ) ;
#6458 = EDGE_CURVE ( 'NONE', #12436, #2275, #10879, .T. ) ;
#6459 = CARTESIAN_POINT ( 'NONE',  ( 235.4000000000000057, 4.447920636657316074, -2.686261716586451520 ) ) ;
#6460 = DIRECTION ( 'NONE',  ( 0.000000000000000000, 1.000000000000000000, 0.000000000000000000 ) ) ;
#6461 = DIRECTION ( 'NONE',  ( 0.000000000000000000, 1.000000000000000000, 0.000000000000000000 ) ) ;
#6462 = AXIS2_PLACEMENT_3D ( 'NONE', #880, #9939, #6886 ) ;
#6463 = DIRECTION ( 'NONE',  ( -0.6368676505102706109, 0.000000000000000000, -0.7709731485165535192 ) ) ;
#6464 = AXIS2_PLACEMENT_3D ( 'NONE', #11089, #4015, #12288 ) ;
#6465 = CARTESIAN_POINT ( 'NONE',  ( 239.0693672988234653, -0.6815372136754875854, 3.433431997329027041 ) ) ;
#6466 = CARTESIAN_POINT ( 'NONE',  ( 14.31396777367018558, -138.4705547276867321, 39.32730324096152685 ) ) ;
#6467 = ADVANCED_FACE ( 'NONE', ( #10950 ), #1820, .F. ) ;
#6468 = CARTESIAN_POINT ( 'NONE',  ( -229.7195872777370198, 3.900365664305255997, -11.35467465479823268 ) ) ;
#6469 = ITEM_DEFINED_TRANSFORMATION ( 'NONE', 'NONE', #11084,  #805 ) ;
#6470 = CIRCLE ( 'NONE', #12842, 2.900000000000000355 ) ;
#6471 = AXIS2_PLACEMENT_3D ( 'NONE', #7636, #3429, #11777 ) ;
#6472 = DIRECTION ( 'NONE',  ( 0.000000000000000000, 0.000000000000000000, 1.000000000000000000 ) ) ;
#6473 = AXIS2_PLACEMENT_3D ( 'NONE', #7750, #6695, #10748 ) ;
#6474 = ORIENTED_EDGE ( 'NONE', *, *, #7766, .F. ) ;
#6475 = CARTESIAN_POINT ( 'NONE',  ( 130.8783844628973441, 19.96883745980737501, -226.6392846544037809 ) ) ;
#6476 = FACE_OUTER_BOUND ( 'NONE', #4248, .T. ) ;
#6477 = DIRECTION ( 'NONE',  ( 8.659560562354926695E-17, 0.7071067811865480168, -0.7071067811865470176 ) ) ;
#6478 = CARTESIAN_POINT ( 'NONE',  ( 122.2593324768346008, 19.00000000000000000, 168.2755348299889988 ) ) ;
#6479 = CARTESIAN_POINT ( 'NONE',  ( -91.83222442980293465, 20.08915143297736705, 243.9837273761026779 ) ) ;
#6480 = TOROIDAL_SURFACE ( 'NONE', #8185, 2.750000000000000000, 0.8000000000000000444 ) ;
#6481 = DIRECTION ( 'NONE',  ( 0.000000000000000000, 0.9998057603070481525, -0.01970892327970899874 ) ) ;
#6482 = DIRECTION ( 'NONE',  ( -0.2588190451025246808, 0.000000000000000000, 0.9659258262890672020 ) ) ;
#6483 = VECTOR ( 'NONE', #5463, 1000.000000000000000 ) ;
#6484 = ADVANCED_FACE ( 'NONE', ( #12686 ), #12682, .F. ) ;
#6485 = CONTEXT_DEPENDENT_SHAPE_REPRESENTATION ( #153, #11768 ) ;
#6486 = EDGE_CURVE ( 'NONE', #4412, #2618, #8644, .T. ) ;
#6487 = CARTESIAN_POINT ( 'NONE',  ( 240.6075165363166093, -3.437532598149585450, -0.7648284531270139741 ) ) ;
#6488 = DIRECTION ( 'NONE',  ( -0.6368676505102707219, 0.000000000000000000, -0.7709731485165536302 ) ) ;
#6489 = ORIENTED_EDGE ( 'NONE', *, *, #9910, .T. ) ;
#6490 = VERTEX_POINT ( 'NONE', #7017 ) ;
#6491 = VECTOR ( 'NONE', #8187, 1000.000000000000000 ) ;
#6492 = EDGE_CURVE ( 'NONE', #4809, #3483, #10137, .T. ) ;
#6493 = CARTESIAN_POINT ( 'NONE',  ( 197.8197553893915028, 30.00000000000000000, -64.27553482998990830 ) ) ;
#6494 = CARTESIAN_POINT ( 'NONE',  ( 185.9653539490014111, -18.00000000000000000, 225.1241593668316625 ) ) ;
#6495 = CONICAL_SURFACE ( 'NONE', #12865, 5.100000000000000533, 0.7853981633974503884 ) ;
#6496 = CARTESIAN_POINT ( 'NONE',  ( 226.6392846536925276, 19.96883745972948176, 130.8783844628973441 ) ) ;
#6497 = DIRECTION ( 'NONE',  ( -0.000000000000000000, -1.000000000000000000, 0.000000000000000000 ) ) ;
#6498 = CARTESIAN_POINT ( 'NONE',  ( 0.000000000000000000, 0.000000000000000000, 0.000000000000000000 ) ) ;
#6499 = CARTESIAN_POINT ( 'NONE',  ( -185.9653539489998195, -30.00000000000000000, -225.1241593668329699 ) ) ;
#6500 = CARTESIAN_POINT ( 'NONE',  ( -178.3611219674587858, 20.79694577634646535, 190.4297758776776277 ) ) ;
#6501 = AXIS2_PLACEMENT_3D ( 'NONE', #7266, #5395, #9268 ) ;
#6502 = EDGE_CURVE ( 'NONE', #3121, #11054, #2128, .T. ) ;
#6503 = EDGE_LOOP ( 'NONE', ( #7561, #6878, #3879, #7157 ) ) ;
#6504 = CARTESIAN_POINT ( 'NONE',  ( 107.6783259591027786, 20.79694577634646535, -237.6585102388687289 ) ) ;
#6505 = EDGE_LOOP ( 'NONE', ( #11918, #10951, #235, #6374 ) ) ;
#6506 = CARTESIAN_POINT ( 'NONE',  ( 0.000000000000000000, 0.000000000000000000, 0.000000000000000000 ) ) ;
#6507 = ORIENTED_EDGE ( 'NONE', *, *, #2624, .T. ) ;
#6508 = ORIENTED_EDGE ( 'NONE', *, *, #7960, .T. ) ;
#6509 = AXIS2_PLACEMENT_3D ( 'NONE', #1327, #1200, #8400 ) ;
#6510 = CARTESIAN_POINT ( 'NONE',  ( 0.000000000000000000, 1.848645179567965036, -239.8169934640518193 ) ) ;
#6511 = PRODUCT_DEFINITION_SHAPE ( 'NONE', 'NONE',  #13051 ) ;
#6512 = DIRECTION ( 'NONE',  ( 0.6368676505102716101, 0.000000000000000000, 0.7709731485165527420 ) ) ;
#6513 = CIRCLE ( 'NONE', #12468, 5.099999999999993427 ) ;
#6514 = DIRECTION ( 'NONE',  ( 0.000000000000000000, 0.000000000000000000, 1.000000000000000000 ) ) ;
#6515 = CARTESIAN_POINT ( 'NONE',  ( -239.3015052057552623, 1.606977719895358092, -11.63957048466796351 ) ) ;
#6516 =( NAMED_UNIT ( * ) PLANE_ANGLE_UNIT ( ) SI_UNIT ( $, .RADIAN. ) );
#6517 = ORIENTED_EDGE ( 'NONE', *, *, #3005, .T. ) ;
#6518 = FACE_OUTER_BOUND ( 'NONE', #6105, .T. ) ;
#6519 = AXIS2_PLACEMENT_3D ( 'NONE', #3513, #9644, #7585 ) ;
#6520 = ORIENTED_EDGE ( 'NONE', *, *, #6741, .F. ) ;
#6521 = DIRECTION ( 'NONE',  ( 0.000000000000000000, 1.000000000000000000, 0.000000000000000000 ) ) ;
#6522 = DIRECTION ( 'NONE',  ( -0.000000000000000000, -1.000000000000000000, 0.000000000000000000 ) ) ;
#6523 = DIRECTION ( 'NONE',  ( 0.000000000000000000, 0.000000000000000000, 1.000000000000000000 ) ) ;
#6524 = CARTESIAN_POINT ( 'NONE',  ( 227.3999999999999773, -0.1024105694488001289, -5.195143123655522110 ) ) ;
#6525 = CARTESIAN_POINT ( 'NONE',  ( -239.3529291969095425, 1.679452495051852789, 11.88190773406936884 ) ) ;
#6526 = CARTESIAN_POINT ( 'NONE',  ( -229.7195242555831385, 3.042667911008530623, 11.35573322796902396 ) ) ;
#6527 = DIRECTION ( 'NONE',  ( 1.000000000000000000, 0.000000000000000000, 0.000000000000000000 ) ) ;
#6528 = APPLICATION_PROTOCOL_DEFINITION ( 'draft international standard', 'automotive_design', 1998, #12327 ) ;
#6529 = EDGE_CURVE ( 'NONE', #1416, #10031, #557, .T. ) ;
#6530 = CARTESIAN_POINT ( 'NONE',  ( -229.7325401777437435, 4.600266235519089975, 11.08951027562286384 ) ) ;
#6531 = EDGE_CURVE ( 'NONE', #3706, #12702, #6943, .T. ) ;
#6532 = ITEM_DEFINED_TRANSFORMATION ( 'NONE', 'NONE', #10222,  #805 ) ;
#6533 = LINE ( 'NONE', #2583, #12118 ) ;
#6534 = ORIENTED_EDGE ( 'NONE', *, *, #12587, .T. ) ;
#6535 =( REPRESENTATION_RELATIONSHIP ('NONE','NONE', #12019, #5191 ) REPRESENTATION_RELATIONSHIP_WITH_TRANSFORMATION ( #3466 )SHAPE_REPRESENTATION_RELATIONSHIP( ) );
#6536 = CARTESIAN_POINT ( 'NONE',  ( 259.4723857435290597, 19.96883745944077404, 34.18476129351889625 ) ) ;
#6537 = CARTESIAN_POINT ( 'NONE',  ( 0.000000000000000000, 21.50000000000000000, -249.7999999999999829 ) ) ;
#6538 = FACE_OUTER_BOUND ( 'NONE', #8239, .T. ) ;
#6539 = PRODUCT_DEFINITION_SHAPE ( 'NONE', 'NONE',  #13170 ) ;
#6540 = PRODUCT_DEFINITION ( 'UNKNOWN', '', #2769, #10416 ) ;
#6541 = CARTESIAN_POINT ( 'NONE',  ( -197.8197553893909912, 19.00000000000000000, 58.77553482999130807 ) ) ;
#6542 = CARTESIAN_POINT ( 'NONE',  ( -115.3046144132258917, 20.08915143297736705, 233.8077470125388970 ) ) ;
#6543 = DIRECTION ( 'NONE',  ( 0.000000000000000000, 0.000000000000000000, 1.000000000000000000 ) ) ;
#6544 = VECTOR ( 'NONE', #3275, 1000.000000000000114 ) ;
#6545 = CARTESIAN_POINT ( 'NONE',  ( -39.32730324096127816, -138.4705547276867321, -14.31396777367084283 ) ) ;
#6546 = LINE ( 'NONE', #1280, #10338 ) ;
#6547 = CONTEXT_DEPENDENT_SHAPE_REPRESENTATION ( #11304, #3991 ) ;
#6548 = CARTESIAN_POINT ( 'NONE',  ( -242.1349625642079388, -6.437046975752621414, -10.12773524509340284 ) ) ;
#6549 = CONICAL_SURFACE ( 'NONE', #5908, 230.0000000000000000, 0.7853981633974476129 ) ;
#6550 = CYLINDRICAL_SURFACE ( 'NONE', #7708, 230.0000000000000000 ) ;
#6551 = VERTEX_POINT ( 'NONE', #4461 ) ;
#6552 = ORIENTED_EDGE ( 'NONE', *, *, #7598, .F. ) ;
#6553 = FACE_OUTER_BOUND ( 'NONE', #9437, .T. ) ;
#6554 = CARTESIAN_POINT ( 'NONE',  ( 227.3999999999999773, -2.999417280921144346, 0.05912676983912736745 ) ) ;
#6555 = EDGE_CURVE ( 'NONE', #5526, #8820, #6546, .T. ) ;
#6556 = EDGE_CURVE ( 'NONE', #5893, #11136, #4583, .T. ) ;
#6557 = CARTESIAN_POINT ( 'NONE',  ( 172.5787240287708073, 19.96883745935533838, 196.7513681801829932 ) ) ;
#6558 = CIRCLE ( 'NONE', #593, 10.00000000000000888 ) ;
#6559 = DIRECTION ( 'NONE',  ( 0.000000000000000000, 0.9998057603070480415, -0.01970892327970899874 ) ) ;
#6560 = DIRECTION ( 'NONE',  ( -0.9961946980917452121, 0.000000000000000000, -0.08715574274766177409 ) ) ;
#6561 =( REPRESENTATION_RELATIONSHIP ('NONE','NONE', #12019, #5191 ) REPRESENTATION_RELATIONSHIP_WITH_TRANSFORMATION ( #3448 )SHAPE_REPRESENTATION_RELATIONSHIP( ) );
#6562 = DIRECTION ( 'NONE',  ( 0.000000000000000000, -0.7071067811864890640, -0.7071067811866059705 ) ) ;
#6563 = CARTESIAN_POINT ( 'NONE',  ( -83.86521783953236309, 20.79694577634646890, 247.0684411393754942 ) ) ;
#6564 = ORIENTED_EDGE ( 'NONE', *, *, #2923, .F. ) ;
#6565 = CARTESIAN_POINT ( 'NONE',  ( 258.6823826759385838, 20.79694577634646890, -34.05310945291962099 ) ) ;
#6566 = ORIENTED_EDGE ( 'NONE', *, *, #12916, .T. ) ;
#6567 = CARTESIAN_POINT ( 'NONE',  ( -161.8917567597108587, -25.00000000000000000, -195.9813743529078636 ) ) ;
#6568 = EDGE_LOOP ( 'NONE', ( #6405, #4550, #8840, #7917 ) ) ;
#6569 = VERTEX_POINT ( 'NONE', #282 ) ;
#6570 = DIRECTION ( 'NONE',  ( -0.4503334343941595708, -0.7071067811865430208, -0.5451603414288016536 ) ) ;
#6571 = ADVANCED_FACE ( 'NONE', ( #1213 ), #7976, .T. ) ;
#6572 = DIRECTION ( 'NONE',  ( 0.000000000000000000, 0.9998057603070481525, -0.01970892327970899874 ) ) ;
#6573 = CARTESIAN_POINT ( 'NONE',  ( 239.3580835734670700, 1.327753754258439889, -3.239279126375866458 ) ) ;
#6574 = CARTESIAN_POINT ( 'NONE',  ( -239.4550024016175769, 1.775410295146655493, -11.61533115162393592 ) ) ;
#6575 = CARTESIAN_POINT ( 'NONE',  ( 0.000000000000000000, -20.00000000000000000, 0.000000000000000000 ) ) ;
#6576 = DIRECTION ( 'NONE',  ( 0.000000000000000000, 1.000000000000000000, 0.000000000000000000 ) ) ;
#6577 = AXIS2_PLACEMENT_3D ( 'NONE', #3238, #323, #7319 ) ;
#6578 = AXIS2_PLACEMENT_3D ( 'NONE', #12678, #3538, #11683 ) ;
#6579 = EDGE_CURVE ( 'NONE', #9887, #7619, #1167, .T. ) ;
#6580 = VECTOR ( 'NONE', #4197, 1000.000000000000000 ) ;
#6581 = AXIS2_PLACEMENT_3D ( 'NONE', #348, #3530, #7540 ) ;
#6582 = ORIENTED_EDGE ( 'NONE', *, *, #4271, .T. ) ;
#6583 = CARTESIAN_POINT ( 'NONE',  ( -238.9094463865829709, -0.9709988936793297887, 11.70980984558256388 ) ) ;
#6584 = VERTEX_POINT ( 'NONE', #12415 ) ;
#6585 = DIRECTION ( 'NONE',  ( -0.6368676505102707219, 0.000000000000000000, -0.7709731485165535192 ) ) ;
#6586 = DIRECTION ( 'NONE',  ( 1.000000000000000000, 0.000000000000000000, 0.000000000000000000 ) ) ;
#6587 = AXIS2_PLACEMENT_3D ( 'NONE', #7259, #1057, #5115 ) ;
#6588 = CARTESIAN_POINT ( 'NONE',  ( 7.347880794884120722E-16, 29.00000000000000000, -213.5000000000000000 ) ) ;
#6589 = FACE_OUTER_BOUND ( 'NONE', #8502, .T. ) ;
#6590 = CARTESIAN_POINT ( 'NONE',  ( -239.3907828020602153, 1.719565078627272259, 11.87615879295651311 ) ) ;
#6591 = CARTESIAN_POINT ( 'NONE',  ( -0.000000000000000000, -9.830508068730530624, 0.000000000000000000 ) ) ;
#6592 = CIRCLE ( 'NONE', #9165, 254.1999999999999886 ) ;
#6593 = CARTESIAN_POINT ( 'NONE',  ( -245.8615520224613249, -9.158310437683550020, 7.754087231521529233 ) ) ;
#6594 = CIRCLE ( 'NONE', #6160, 2.000000000000000444 ) ;
#6595 = LINE ( 'NONE', #9772, #6934 ) ;
#6596 = DIRECTION ( 'NONE',  ( 0.9848077530122103518, 0.000000000000000000, -0.1736481776669172583 ) ) ;
#6597 = CARTESIAN_POINT ( 'NONE',  ( 159.3442861576696714, 11.79660968244693997, 192.8974817588417068 ) ) ;
#6598 = ITEM_DEFINED_TRANSFORMATION ( 'NONE', 'NONE', #7254,  #805 ) ;
#6599 = VERTEX_POINT ( 'NONE', #8417 ) ;
#6600 = CARTESIAN_POINT ( 'NONE',  ( 235.0999999999999943, 1.949621232598743648, -0.03843240039543253939 ) ) ;
#6601 = VERTEX_POINT ( 'NONE', #8545 ) ;
#6602 = CARTESIAN_POINT ( 'NONE',  ( -261.1558126970361400, 19.96883746053716990, -17.09264059830048410 ) ) ;
#6603 = DIRECTION ( 'NONE',  ( 0.000000000000000000, 0.01970892327970899874, 0.9998057603070481525 ) ) ;
#6604 = DIRECTION ( 'NONE',  ( -0.6368676505102707219, 0.000000000000000000, -0.7709731485165535192 ) ) ;
#6605 =( REPRESENTATION_RELATIONSHIP ('NONE','NONE', #12019, #182 ) REPRESENTATION_RELATIONSHIP_WITH_TRANSFORMATION ( #7986 )SHAPE_REPRESENTATION_RELATIONSHIP( ) );
#6606 = EDGE_CURVE ( 'NONE', #7625, #6775, #349, .T. ) ;
#6607 = DIRECTION ( 'NONE',  ( 0.000000000000000000, -0.9998057603070480415, 0.01970892327970911323 ) ) ;
#6608 = CARTESIAN_POINT ( 'NONE',  ( -181.8257142206830679, -18.00000000000000000, -220.1128339014753692 ) ) ;
#6609 = B_SPLINE_CURVE_WITH_KNOTS ( 'NONE', 3,
 ( #8240, #11163, #3281, #11225, #10290, #10224, #5362, #1169, #9433, #2160, #5290, #12295, #5153, #6305, #168, #2031, #4222, #3344, #10354, #38, #1230, #8371, #9365, #10153, #6102, #12432, #304, #4359, #1028, #4093, #8172, #3088, #7166, #9612, #498, #6565, #2486, #2360, #1427, #12688, #4546, #4608, #3615, #11566, #8629, #6435, #9546, #3548, #365, #10497, #5488, #1365, #7620, #1558, #2423, #5622, #6504, #432, #8565, #7496, #6629, #12621, #4413, #11634, #8684, #10560 ),
 .UNSPECIFIED., .F., .F.,
 ( 4, 2, 2, 2, 2, 2, 2, 2, 2, 2, 2, 2, 2, 2, 2, 2, 2, 2, 2, 2, 2, 2, 2, 2, 2, 2, 2, 2, 2, 2, 2, 2, 4 ),
 ( 0.000000000000000000, 0.01562499999999998265, 0.03124999999999996531, 0.04687499999999994449, 0.06249999999999993061, 0.07812499999999991673, 0.09374999999999991673, 0.1093749999999999306, 0.1249999999999999445, 0.1406249999999999445, 0.1562499999999999722, 0.1718749999999999722, 0.1874999999999999722, 0.2031250000000000000, 0.2187500000000000000, 0.2343750000000000278, 0.2500000000000000555, 0.2656250000000000555, 0.2812500000000000000, 0.2968750000000000000, 0.3125000000000000000, 0.3281249999999999445, 0.3437499999999999445, 0.3593749999999999445, 0.3749999999999998890, 0.3906249999999998890, 0.4062499999999998890, 0.4218749999999998890, 0.4374999999999998890, 0.4531249999999999445, 0.4687500000000000000, 0.4843750000000000000, 0.5000000000000000000 ),
 .UNSPECIFIED. ) ;
#6610 = DIRECTION ( 'NONE',  ( 0.6368676505102696117, 0.000000000000000000, 0.7709731485165545184 ) ) ;
#6611 = DIRECTION ( 'NONE',  ( 0.4999999999999980016, 0.000000000000000000, 0.8660254037844398178 ) ) ;
#6612 = CARTESIAN_POINT ( 'NONE',  ( 229.9996470147345349, 3.477012619071095934, -0.4608790345419201406 ) ) ;
#6613 = CONTEXT_DEPENDENT_SHAPE_REPRESENTATION ( #10696, #584 ) ;
#6614 = DIRECTION ( 'NONE',  ( -0.000000000000000000, -1.000000000000000000, 0.000000000000000000 ) ) ;
#6615 = CARTESIAN_POINT ( 'NONE',  ( -229.8662995960750379, -9.087301588047655088, 7.845977234077500917 ) ) ;
#6616 = EDGE_LOOP ( 'NONE', ( #12988, #11891, #1382, #8070 ) ) ;
#6617 = ORIENTED_EDGE ( 'NONE', *, *, #6973, .T. ) ;
#6618 = AXIS2_PLACEMENT_3D ( 'NONE', #7729, #6744, #801 ) ;
#6619 = CARTESIAN_POINT ( 'NONE',  ( 3.059167704270088292E-14, 11.79660968244690089, -249.7999999999999829 ) ) ;
#6620 = FACE_BOUND ( 'NONE', #1984, .T. ) ;
#6621 = ADVANCED_FACE ( 'NONE', ( #9281 ), #7558, .T. ) ;
#6622 = CARTESIAN_POINT ( 'NONE',  ( 259.6535381495586421, 20.55460285116648578, 34.20858920465607156 ) ) ;
#6623 = CARTESIAN_POINT ( 'NONE',  ( -289.8128292627096130, -30.00000000000000000, 10.41748504886635907 ) ) ;
#6624 = CARTESIAN_POINT ( 'NONE',  ( 0.000000000000000000, 0.000000000000000000, 0.000000000000000000 ) ) ;
#6625 = CYLINDRICAL_SURFACE ( 'NONE', #12628, 5.500000000000005329 ) ;
#6626 = DIRECTION ( 'NONE',  ( 0.6368676505102689456, 0.000000000000000000, 0.7709731485165549625 ) ) ;
#6627 = DIRECTION ( 'NONE',  ( 0.000000000000000000, 0.9998057603070481525, -0.01970892327970899874 ) ) ;
#6628 = ORIENTED_EDGE ( 'NONE', *, *, #5254, .F. ) ;
#6629 = CARTESIAN_POINT ( 'NONE',  ( 59.24444182677506632, 20.79694577634646180, -254.0989678903618483 ) ) ;
#6630 = EDGE_CURVE ( 'NONE', #7040, #10564, #1344, .T. ) ;
#6631 = ORIENTED_EDGE ( 'NONE', *, *, #3577, .T. ) ;
#6632 = ADVANCED_FACE ( 'NONE', ( #8479 ), #4204, .F. ) ;
#6633 = DIRECTION ( 'NONE',  ( 0.6368676505102709440, 0.000000000000000000, 0.7709731485165532971 ) ) ;
#6634 = ORIENTED_EDGE ( 'NONE', *, *, #11991, .F. ) ;
#6635 = ORIENTED_EDGE ( 'NONE', *, *, #4125, .F. ) ;
#6636 = CIRCLE ( 'NONE', #5355, 6.500000000000000000 ) ;
#6637 = CARTESIAN_POINT ( 'NONE',  ( 71.82423009839129691, 18.00000000000000000, -197.3354503650404865 ) ) ;
#6638 = AXIS2_PLACEMENT_3D ( 'NONE', #4903, #10040, #6046 ) ;
#6639 = CARTESIAN_POINT ( 'NONE',  ( 239.2334266250973940, 1.105838440818801116, 3.321566349753109382 ) ) ;
#6640 = DIRECTION ( 'NONE',  ( 0.000000000000000000, -1.000000000000000000, 0.000000000000000000 ) ) ;
#6641 = CARTESIAN_POINT ( 'NONE',  ( -172.1812796675209825, 20.08915143307664053, -196.2980642830465001 ) ) ;
#6642 = FACE_OUTER_BOUND ( 'NONE', #611, .T. ) ;
#6643 =( NAMED_UNIT ( * ) PLANE_ANGLE_UNIT ( ) SI_UNIT ( $, .RADIAN. ) );
#6644 = B_SPLINE_CURVE_WITH_KNOTS ( 'NONE', 3,
 ( #10268, #5581, #210, #12710, #12343, #4200, #9643, #11341, #11657, #11411, #2208, #6284, #277, #10334, #5270, #525, #9341, #4268, #2267, #6345, #1275, #8654, #8413, #5340, #3325, #2511, #4333, #12474, #7584, #6593, #3574, #7646, #1644, #2897, #4703, #784, #12588, #10844, #1716, #7983, #8849, #5985, #4774, #7777, #11040, #1914, #7841, #12910, #2763, #10910, #10044, #723, #2637, #12046, #2697, #1788, #3841, #9979, #8781, #3713, #11913, #5783, #6850, #10980, #9843, #6921, #3772, #4908, #5854, #6981, #5712, #9912, #3909, #4834, #9771, #6726, #850, #8917, #9046, #7909, #8047, #12846, #1852, #12978, #916, #11981, #11850, #2832, #652, #5916, #8981, #4974, #6419, #3971, #10778, #6787, #11175 ),
 .UNSPECIFIED., .F., .F.,
 ( 4, 1, 1, 2, 2, 2, 1, 1, 1, 2, 2, 2, 2, 1, 1, 1, 2, 2, 2, 1, 1, 1, 2, 2, 2, 1, 1, 1, 1, 2, 2, 2, 1, 1, 1, 2, 2, 1, 1, 1, 1, 2, 2, 2, 2, 1, 1, 1, 2, 2, 2, 2, 1, 1, 1, 2, 2, 2, 1, 1, 1, 2, 2, 4 ),
 ( 0.000000000000000000, 0.03125000000007535639, 0.04687500000011302070, 0.05468750000013182511, 0.06250000000015062951, 0.09375000000022588875, 0.1093750000002635253, 0.1171875000002850359, 0.1210937500002958050, 0.1230468750003012174, 0.1250000000003066158, 0.1875000000002915723, 0.2187500000002840506, 0.2343750000002802203, 0.2421875000002760014, 0.2460937500002739475, 0.2480468750002728928, 0.2500000000002718381, 0.2812500000002386980, 0.2968750000002220446, 0.3046875000002159939, 0.3085937500002151057, 0.3105468750002147726, 0.3125000000002144396, 0.3437500000002070566, 0.3593750000002033929, 0.3671875000002014500, 0.3710937500002023937, 0.3730468750002007838, 0.3740234375002000067, 0.3750000000001991740, 0.4062500000001449396, 0.4218750000001178502, 0.4296875000001044165, 0.4335937500000993650, 0.4355468750000968114, 0.4375000000000942579, 0.4687500000000812683, 0.4843750000000728306, 0.4921875000000685563, 0.4960937500000662248, 0.4980468750000652256, 0.5000000000000641709, 0.5625000000000439648, 0.5937500000000357492, 0.6093750000000297540, 0.6171875000000246470, 0.6210937500000223155, 0.6230468750000212053, 0.6250000000000199840, 0.6875000000000007772, 0.7187499999999896749, 0.7343749999999842348, 0.7421874999999797939, 0.7460937499999792388, 0.7480468749999805711, 0.7499999999999817923, 0.8125000000000066613, 0.8437500000000190958, 0.8593750000000254241, 0.8671875000000272005, 0.8710937500000280886, 0.8750000000000289768, 1.000000000000000000 ),
 .UNSPECIFIED. ) ;
#6645 = ORIENTED_EDGE ( 'NONE', *, *, #2556, .T. ) ;
#6646 = CARTESIAN_POINT ( 'NONE',  ( -238.9600686717498377, -1.084978034942615244, 11.70002422621010929 ) ) ;
#6647 = EDGE_CURVE ( 'NONE', #1953, #1244, #9256, .T. ) ;
#6648 = VERTEX_POINT ( 'NONE', #12537 ) ;
#6649 = EDGE_CURVE ( 'NONE', #10082, #10483, #9670, .T. ) ;
#6650 = PRODUCT_DEFINITION_SHAPE ( 'NONE', 'NONE',  #13172 ) ;
#6651 = CARTESIAN_POINT ( 'NONE',  ( -242.9139448639247121, 7.229284210467626259, -9.262738307079473543 ) ) ;
#6652 = DIRECTION ( 'NONE',  ( 0.000000000000000000, 1.000000000000000000, 0.000000000000000000 ) ) ;
#6653 = AXIS2_PLACEMENT_3D ( 'NONE', #5600, #7599, #8664 ) ;
#6654 = EDGE_CURVE ( 'NONE', #2131, #11915, #12024, .T. ) ;
#6655 = CARTESIAN_POINT ( 'NONE',  ( 0.000000000000000000, 25.00000000000000000, 0.000000000000000000 ) ) ;
#6656 = CARTESIAN_POINT ( 'NONE',  ( 0.000000000000000000, 30.00000000000000000, 208.0000000000000000 ) ) ;
#6657 = DIRECTION ( 'NONE',  ( 0.6368676505102696117, 0.000000000000000000, 0.7709731485165545184 ) ) ;
#6658 = CIRCLE ( 'NONE', #9618, 6.500000000000005329 ) ;
#6659 = CARTESIAN_POINT ( 'NONE',  ( -229.7429378870860717, 4.500510568802750910, 10.87411266180416547 ) ) ;
#6660 = CARTESIAN_POINT ( 'NONE',  ( 0.000000000000000000, 11.79660968244693997, 0.000000000000000000 ) ) ;
#6661 = DIRECTION ( 'NONE',  ( -0.000000000000000000, -1.000000000000000000, 0.000000000000000000 ) ) ;
#6662 = VECTOR ( 'NONE', #3693, 1000.000000000000114 ) ;
#6663 = CARTESIAN_POINT ( 'NONE',  ( -229.8660307814922987, 9.077839160772928295, 7.850369537300845302 ) ) ;
#6664 = ORIENTED_EDGE ( 'NONE', *, *, #11893, .T. ) ;
#6665 = EDGE_CURVE ( 'NONE', #158, #7755, #3396, .T. ) ;
#6666 = ORIENTED_EDGE ( 'NONE', *, *, #2863, .F. ) ;
#6667 = CARTESIAN_POINT ( 'NONE',  ( -122.2593324768321992, 19.00000000000000000, 173.7755348299905052 ) ) ;
#6668 = VERTEX_POINT ( 'NONE', #9663 ) ;
#6669 = ADVANCED_BREP_SHAPE_REPRESENTATION ( '', ( #10471, #805 ), #5055 ) ;
#6670 = CIRCLE ( 'NONE', #10705, 239.0000000000000000 ) ;
#6671 = CARTESIAN_POINT ( 'NONE',  ( 67.71318189785222330, 19.96883746181513786, 252.8031682274115042 ) ) ;
#6672 = FACE_OUTER_BOUND ( 'NONE', #12871, .T. ) ;
#6673 = PLANE ( 'NONE',  #12640 ) ;
#6674 = CIRCLE ( 'NONE', #1553, 249.7999999999999829 ) ;
#6675 = CARTESIAN_POINT ( 'NONE',  ( -286.5648042451072115, -19.40000000000000213, 14.34944810630078393 ) ) ;
#6676 = DIRECTION ( 'NONE',  ( 0.000000000000000000, 0.000000000000000000, 1.000000000000000000 ) ) ;
#6677 = DIRECTION ( 'NONE',  ( 0.000000000000000000, 1.000000000000000000, 0.000000000000000000 ) ) ;
#6678 = DIRECTION ( 'NONE',  ( -0.2847642722309811636, 0.5538822189107471816, -0.7823834078220643917 ) ) ;
#6679 = VECTOR ( 'NONE', #4295, 1000.000000000000000 ) ;
#6680 = CARTESIAN_POINT ( 'NONE',  ( 229.9996562797466026, 3.477621119227378710, 0.4561944637181986617 ) ) ;
#6681 = TOROIDAL_SURFACE ( 'NONE', #2821, 250.0000000000000000, 10.00000000000000000 ) ;
#6682 = CONTEXT_DEPENDENT_SHAPE_REPRESENTATION ( #11041, #12930 ) ;
#6683 = CIRCLE ( 'NONE', #9225, 1.750000000000000000 ) ;
#6684 = CARTESIAN_POINT ( 'NONE',  ( -249.6784491604725531, 11.18557168014761061, -3.597985675038290587 ) ) ;
#6685 = CARTESIAN_POINT ( 'NONE',  ( -240.2229988806957124, -3.132498172368823219, -11.58475653430379637 ) ) ;
#6686 = DIRECTION ( 'NONE',  ( 1.000000000000000000, 0.000000000000000000, 0.000000000000000000 ) ) ;
#6687 = ORIENTED_EDGE ( 'NONE', *, *, #986, .F. ) ;
#6688 = ORIENTED_EDGE ( 'NONE', *, *, #3579, .T. ) ;
#6689 = DIRECTION ( 'NONE',  ( 0.000000000000000000, 0.000000000000000000, 1.000000000000000000 ) ) ;
#6690 = DIRECTION ( 'NONE',  ( -0.000000000000000000, -1.000000000000000000, 0.000000000000000000 ) ) ;
#6691 = AXIS2_PLACEMENT_3D ( 'NONE', #8835, #5902, #4897 ) ;
#6692 = CARTESIAN_POINT ( 'NONE',  ( 207.7919029858380213, 20.55460285149987953, -159.4136521842188188 ) ) ;
#6693 = FACE_OUTER_BOUND ( 'NONE', #8944, .T. ) ;
#6694 = DIRECTION ( 'NONE',  ( -0.9063077870366510469, 0.000000000000000000, 0.4226182617406972208 ) ) ;
#6695 = DIRECTION ( 'NONE',  ( 0.000000000000000000, 1.000000000000000000, 0.000000000000000000 ) ) ;
#6696 = CARTESIAN_POINT ( 'NONE',  ( 71.82423009839129691, 19.40000000000000213, 197.3354503650404865 ) ) ;
#6697 = VERTEX_POINT ( 'NONE', #5804 ) ;
#6698 = EDGE_CURVE ( 'NONE', #2361, #9366, #9040, .T. ) ;
#6699 = EDGE_CURVE ( 'NONE', #1401, #5843, #4656, .T. ) ;
#6700 = VECTOR ( 'NONE', #8318, 1000.000000000000000 ) ;
#6701 = LINE ( 'NONE', #10687, #2944 ) ;
#6702 = VERTEX_POINT ( 'NONE', #3791 ) ;
#6703 = ORIENTED_EDGE ( 'NONE', *, *, #1396, .T. ) ;
#6704 = CARTESIAN_POINT ( 'NONE',  ( 260.1353576186481291, 20.08915143297736705, 17.05322212017798833 ) ) ;
#6705 = ORIENTED_EDGE ( 'NONE', *, *, #4365, .F. ) ;
#6706 = LINE ( 'NONE', #1766, #8800 ) ;
#6707 = CARTESIAN_POINT ( 'NONE',  ( -239.5361044668155159, 1.848645179572584896, -11.60366368868220022 ) ) ;
#6708 = CARTESIAN_POINT ( 'NONE',  ( -115.4648407707716018, 20.08915143296762906, -234.1947771733659920 ) ) ;
#6709 = VECTOR ( 'NONE', #11549, 1000.000000000000000 ) ;
#6710 = DIRECTION ( 'NONE',  ( 0.000000000000000000, -0.7071067811865489050, -0.7071067811865460184 ) ) ;
#6711 = CARTESIAN_POINT ( 'NONE',  ( 0.000000000000000000, 0.000000000000000000, 0.000000000000000000 ) ) ;
#6712 = DIRECTION ( 'NONE',  ( 0.000000000000000000, 1.000000000000000000, 0.000000000000000000 ) ) ;
#6713 = CONTEXT_DEPENDENT_SHAPE_REPRESENTATION ( #10952, #12822 ) ;
#6714 = ORIENTED_EDGE ( 'NONE', *, *, #6243, .T. ) ;
#6715 = CARTESIAN_POINT ( 'NONE',  ( -249.7118339206215012, -9.997999799959989886, -6.636264009214830395 ) ) ;
#6716 = ORIENTED_EDGE ( 'NONE', *, *, #11027, .F. ) ;
#6717 = DIRECTION ( 'NONE',  ( 0.000000000000000000, -1.000000000000000000, 0.000000000000000000 ) ) ;
#6718 = ORIENTED_EDGE ( 'NONE', *, *, #5128, .F. ) ;
#6719 = CIRCLE ( 'NONE', #10751, 3.000000000000002665 ) ;
#6720 = DIRECTION ( 'NONE',  ( -0.000000000000000000, 1.000000000000000000, 0.000000000000000000 ) ) ;
#6721 = FACE_OUTER_BOUND ( 'NONE', #3912, .T. ) ;
#6722 = DIRECTION ( 'NONE',  ( 0.000000000000000000, -1.000000000000000000, 0.000000000000000000 ) ) ;
#6723 = EDGE_CURVE ( 'NONE', #1001, #4565, #10864, .T. ) ;
#6724 = CARTESIAN_POINT ( 'NONE',  ( -229.8696931595135311, 8.856154740712108620, -7.760084353341174079 ) ) ;
#6725 = EDGE_CURVE ( 'NONE', #4180, #9382, #112, .T. ) ;
#6726 = CARTESIAN_POINT ( 'NONE',  ( -241.9339721712941866, -6.203520525772937333, 10.27503750702521224 ) ) ;
#6727 = AXIS2_PLACEMENT_3D ( 'NONE', #11851, #586, #5651 ) ;
#6728 = CARTESIAN_POINT ( 'NONE',  ( -238.6985546758615442, -1.431921744593627863E-13, 12.00000000011287504 ) ) ;
#6729 = AXIS2_PLACEMENT_3D ( 'NONE', #13032, #9967, #12970 ) ;
#6730 = ORIENTED_EDGE ( 'NONE', *, *, #7292, .T. ) ;
#6731 = CARTESIAN_POINT ( 'NONE',  ( -229.8321229872749143, 8.181811570953646751, 8.792102906095127679 ) ) ;
#6732 = ORIENTED_EDGE ( 'NONE', *, *, #2783, .F. ) ;
#6733 = VERTEX_POINT ( 'NONE', #11064 ) ;
#6734 = CARTESIAN_POINT ( 'NONE',  ( -248.5901226956339372, -9.992747119255737331, -6.181484274823088931 ) ) ;
#6735 = EDGE_LOOP ( 'NONE', ( #6752, #12481, #11531, #8723 ) ) ;
#6736 = CARTESIAN_POINT ( 'NONE',  ( -172.6991790971032970, 20.55460285072942384, -196.8887528238318509 ) ) ;
#6737 = LINE ( 'NONE', #8793, #5297 ) ;
#6738 = CARTESIAN_POINT ( 'NONE',  ( -294.1869546181095529, -19.00000000000000000, -31.92980917095498938 ) ) ;
#6739 =( REPRESENTATION_RELATIONSHIP ('NONE','NONE', #12019, #5191 ) REPRESENTATION_RELATIONSHIP_WITH_TRANSFORMATION ( #9197 )SHAPE_REPRESENTATION_RELATIONSHIP( ) );
#6740 = DIRECTION ( 'NONE',  ( 0.000000000000000000, 0.9998057603070480415, -0.01970892327970899874 ) ) ;
#6741 = EDGE_CURVE ( 'NONE', #12659, #3500, #5429, .T. ) ;
#6742 = DIRECTION ( 'NONE',  ( 0.000000000000000000, -1.000000000000000000, 0.000000000000000000 ) ) ;
#6743 = DIRECTION ( 'NONE',  ( 1.000000000000000000, 0.000000000000000000, 0.000000000000000000 ) ) ;
#6744 = DIRECTION ( 'NONE',  ( 0.2154914511802929478, 0.5538822189107472926, -0.8042250444015772715 ) ) ;
#6745 = CARTESIAN_POINT ( 'NONE',  ( -229.8695287356393351, -8.851891635873659681, -7.764920136789899452 ) ) ;
#6746 = ADVANCED_FACE ( 'NONE', ( #998 ), #5873, .T. ) ;
#6747 = ITEM_DEFINED_TRANSFORMATION ( 'NONE', 'NONE', #6825,  #805 ) ;
#6748 = CARTESIAN_POINT ( 'NONE',  ( -248.8393377457010729, 10.13317597125110225, -5.948217566805436896 ) ) ;
#6749 = FACE_OUTER_BOUND ( 'NONE', #11351, .T. ) ;
#6750 = CARTESIAN_POINT ( 'NONE',  ( -0.000000000000000000, -19.00000000000000000, 0.000000000000000000 ) ) ;
#6751 = EDGE_LOOP ( 'NONE', ( #9333, #5177, #3166, #3104 ) ) ;
#6752 = ORIENTED_EDGE ( 'NONE', *, *, #9689, .F. ) ;
#6753 = DIRECTION ( 'NONE',  ( -0.000000000000000000, -1.000000000000000000, 0.000000000000000000 ) ) ;
#6754 = FACE_OUTER_BOUND ( 'NONE', #12166, .T. ) ;
#6755 = CARTESIAN_POINT ( 'NONE',  ( 115.8123742916068295, 20.55460285108873819, 234.8993005735927966 ) ) ;
#6756 = DIRECTION ( 'NONE',  ( 0.000000000000000000, 0.9998057603070481525, -0.01970892327970899874 ) ) ;
#6757 = PRODUCT_DEFINITION_SHAPE ( 'NONE', 'NONE',  #13173 ) ;
#6758 = DIRECTION ( 'NONE',  ( -0.9396926207859106484, 0.000000000000000000, 0.3420201433256631063 ) ) ;
#6759 = FACE_OUTER_BOUND ( 'NONE', #7334, .T. ) ;
#6760 = CARTESIAN_POINT ( 'NONE',  ( 239.8763759935475548, 1.918973793112176640, -2.928207549571361312 ) ) ;
#6761 = ORIENTED_EDGE ( 'NONE', *, *, #3769, .T. ) ;
#6762 = DIRECTION ( 'NONE',  ( 8.659560562355648996E-17, -0.7071067811864890640, 0.7071067811866059705 ) ) ;
#6763 = EDGE_LOOP ( 'NONE', ( #1814, #7022, #11728, #11048 ) ) ;
#6764 = ORIENTED_EDGE ( 'NONE', *, *, #8442, .F. ) ;
#6765 = CARTESIAN_POINT ( 'NONE',  ( 251.8100110699624281, 20.08915143297736705, 67.47543992452017392 ) ) ;
#6766 = VERTEX_POINT ( 'NONE', #7932 ) ;
#6767 = PRODUCT_DEFINITION_SHAPE ( 'NONE', 'NONE',  #13131 ) ;
#6768 = DIRECTION ( 'NONE',  ( 0.000000000000000000, 1.000000000000000000, 0.000000000000000000 ) ) ;
#6769 = AXIS2_PLACEMENT_3D ( 'NONE', #6994, #8863, #3785 ) ;
#6770 = LINE ( 'NONE', #10760, #10848 ) ;
#6771 = ADVANCED_FACE ( 'NONE', ( #9196 ), #11129, .F. ) ;
#6772 = CARTESIAN_POINT ( 'NONE',  ( 3.039165139883823160E-14, -9.830508068699650437, -248.1666666666509968 ) ) ;
#6773 = DIRECTION ( 'NONE',  ( 0.000000000000000000, 0.7071067811865450192, 0.7071067811865500152 ) ) ;
#6774 = FACE_OUTER_BOUND ( 'NONE', #3147, .T. ) ;
#6775 = VERTEX_POINT ( 'NONE', #802 ) ;
#6776 = DIRECTION ( 'NONE',  ( 0.000000000000000000, 1.000000000000000000, 0.000000000000000000 ) ) ;
#6778 = ORIENTED_EDGE ( 'NONE', *, *, #5837, .T. ) ;
#6777 = AXIS2_PLACEMENT_3D ( 'NONE', #5549, #12616, #7616 ) ;
#6779 = CARTESIAN_POINT ( 'NONE',  ( -243.1520458356562528, 7.443371746708626446, -9.091683909951978393 ) ) ;
#6780 = ORIENTED_EDGE ( 'NONE', *, *, #2512, .F. ) ;
#6781 = DIRECTION ( 'NONE',  ( 0.000000000000000000, 1.000000000000000000, 0.000000000000000000 ) ) ;
#6782 = DIRECTION ( 'NONE',  ( -0.6368676505102700558, 0.000000000000000000, -0.7709731485165541853 ) ) ;
#6783 = CARTESIAN_POINT ( 'NONE',  ( -249.7118339206215012, -9.997999799959989886, 6.636264009214830395 ) ) ;
#6784 = CIRCLE ( 'NONE', #10817, 5.100000000000003197 ) ;
#6785 = PLANE ( 'NONE',  #163 ) ;
#6786 = AXIS2_PLACEMENT_3D ( 'NONE', #2668, #5952, #11880 ) ;
#6787 = CARTESIAN_POINT ( 'NONE',  ( -240.0746691521297578, -2.719637366637591036, 11.70176364698651561 ) ) ;
#6788 = CARTESIAN_POINT ( 'NONE',  ( -238.7054772606637414, 0.2144843524526476863, -11.99854086871946635 ) ) ;
#6789 = VERTEX_POINT ( 'NONE', #1935 ) ;
#6790 = DIRECTION ( 'NONE',  ( 0.000000000000000000, 1.000000000000000000, 0.000000000000000000 ) ) ;
#6791 = CONTEXT_DEPENDENT_SHAPE_REPRESENTATION ( #1104, #4715 ) ;
#6792 = ORIENTED_EDGE ( 'NONE', *, *, #5815, .T. ) ;
#6793 = EDGE_CURVE ( 'NONE', #941, #1921, #6282, .T. ) ;
#6794 = PRODUCT_DEFINITION_SHAPE ( 'NONE', 'NONE',  #8087 ) ;
#6795 = EDGE_CURVE ( 'NONE', #8227, #10637, #3860, .T. ) ;
#6796 = ORIENTED_EDGE ( 'NONE', *, *, #12176, .T. ) ;
#6797 = AXIS2_PLACEMENT_3D ( 'NONE', #7184, #9056, #187 ) ;
#6798 = CARTESIAN_POINT ( 'NONE',  ( 259.6535381495586421, 20.55460285116648578, 34.20858920465607156 ) ) ;
#6799 = PLANE ( 'NONE',  #12745 ) ;
#6800 = DIRECTION ( 'NONE',  ( 1.000000000000000000, 0.000000000000000000, 0.000000000000000000 ) ) ;
#6801 = AXIS2_PLACEMENT_3D ( 'NONE', #10587, #1460, #5525 ) ;
#6802 = CYLINDRICAL_SURFACE ( 'NONE', #8099, 230.0000000000000000 ) ;
#6803 = CARTESIAN_POINT ( 'NONE',  ( -240.2963067560768025, 3.341048620542326208, 11.52705098701326847 ) ) ;
#6804 = AXIS2_PLACEMENT_3D ( 'NONE', #8113, #7044, #1721 ) ;
#6805 = CARTESIAN_POINT ( 'NONE',  ( 0.000000000000000000, 0.000000000000000000, 0.000000000000000000 ) ) ;
#6806 = DIRECTION ( 'NONE',  ( 0.07256543843576360175, 0.5538822189107471816, -0.8294267566935205060 ) ) ;
#6807 = CARTESIAN_POINT ( 'NONE',  ( 229.9800038605684733, 1.757442049980142862, 3.035487404091129271 ) ) ;
#6808 = CONICAL_SURFACE ( 'NONE', #8513, 5.500000000000015099, 0.7853981633974461696 ) ;
#6809 = CARTESIAN_POINT ( 'NONE',  ( -249.7762712554156224, 11.55521436326935003, 2.133810498956889123 ) ) ;
#6810 = CARTESIAN_POINT ( 'NONE',  ( -242.2936178119639123, -6.614827065997419098, -10.01219624237291761 ) ) ;
#6811 = EDGE_CURVE ( 'NONE', #4597, #2702, #6941, .T. ) ;
#6812 = LINE ( 'NONE', #12066, #5805 ) ;
#6813 = ORIENTED_EDGE ( 'NONE', *, *, #1353, .T. ) ;
#6814 = ORIENTED_EDGE ( 'NONE', *, *, #9012, .T. ) ;
#6815 = VECTOR ( 'NONE', #2431, 1000.000000000000000 ) ;
#6816 = CARTESIAN_POINT ( 'NONE',  ( -83.95474316043620888, 20.08915143278693094, 247.2466869562449858 ) ) ;
#6817 = CARTESIAN_POINT ( 'NONE',  ( -225.1241593668336236, -19.00000000000000000, 185.9653539489990521 ) ) ;
#6818 = EDGE_CURVE ( 'NONE', #9288, #2131, #9068, .T. ) ;
#6819 = CARTESIAN_POINT ( 'NONE',  ( 17.06760680800665142, 20.79694577634646180, -260.7745447061710138 ) ) ;
#6820 = DIRECTION ( 'NONE',  ( 1.000000000000000000, 0.000000000000000000, 0.000000000000000000 ) ) ;
#6821 = DIRECTION ( 'NONE',  ( 0.9659258262890708657, 0.000000000000000000, -0.2588190451025111916 ) ) ;
#6822 = DIRECTION ( 'NONE',  ( 0.000000000000000000, 1.000000000000000000, 0.000000000000000000 ) ) ;
#6823 = CARTESIAN_POINT ( 'NONE',  ( 240.3826708216974737, 2.772967769358989809, -2.135567781667440102 ) ) ;
#6824 = ORIENTED_EDGE ( 'NONE', *, *, #1901, .F. ) ;
#6825 = AXIS2_PLACEMENT_3D ( 'NONE', #8799, #12999, #5872 ) ;
#6826 = CARTESIAN_POINT ( 'NONE',  ( 0.000000000000000000, -1.848645179579245124, 0.000000000000000000 ) ) ;
#6827 = EDGE_LOOP ( 'NONE', ( #1705, #12022, #6507, #10783 ) ) ;
#6828 = VERTEX_POINT ( 'NONE', #10185 ) ;
#6829 = DIRECTION ( 'NONE',  ( 0.4503334343941441387, 0.7071067811865670016, 0.5451603414287832239 ) ) ;
#6830 = ORIENTED_EDGE ( 'NONE', *, *, #11373, .T. ) ;
#6831 = CARTESIAN_POINT ( 'NONE',  ( 220.3999999999999773, 0.000000000000000000, 0.000000000000000000 ) ) ;
#6832 = CARTESIAN_POINT ( 'NONE',  ( -158.9353507248835058, 20.08915143316258778, 207.1687172305619811 ) ) ;
#6833 = PRODUCT_DEFINITION_FORMATION_WITH_SPECIFIED_SOURCE ( 'ANY', '', #1393, .NOT_KNOWN. ) ;
#6834 = CARTESIAN_POINT ( 'NONE',  ( 197.8197553893915028, 30.00000000000000000, -69.77553482998990830 ) ) ;
#6835 = LINE ( 'NONE', #8766, #11348 ) ;
#6836 = ORIENTED_EDGE ( 'NONE', *, *, #4554, .F. ) ;
#6837 = CARTESIAN_POINT ( 'NONE',  ( -0.000000000000000000, -21.50000000000000000, 0.000000000000000000 ) ) ;
#6838 = VERTEX_POINT ( 'NONE', #4 ) ;
#6839 = CARTESIAN_POINT ( 'NONE',  ( -238.9989076641871861, 1.159495722235804216, 11.69268798918628249 ) ) ;
#6840 = ORIENTED_EDGE ( 'NONE', *, *, #535, .T. ) ;
#6841 = EDGE_CURVE ( 'NONE', #12029, #3737, #7342, .T. ) ;
#6842 = AXIS2_PLACEMENT_3D ( 'NONE', #4699, #9635, #10711 ) ;
#6843 = DIRECTION ( 'NONE',  ( -0.000000000000000000, -1.000000000000000000, 0.000000000000000000 ) ) ;
#6844 = CARTESIAN_POINT ( 'NONE',  ( -238.7109915777814138, -2.671037648644427152E-08, -11.74999999995326050 ) ) ;
#6845 = DIRECTION ( 'NONE',  ( -0.000000000000000000, -1.000000000000000000, 0.000000000000000000 ) ) ;
#6846 = CARTESIAN_POINT ( 'NONE',  ( -249.7380656782638368, -10.65316887766604381, 5.649205583156061472 ) ) ;
#6847 = DIRECTION ( 'NONE',  ( 1.000000000000000000, 0.000000000000000000, 0.000000000000000000 ) ) ;
#6848 = AXIS2_PLACEMENT_3D ( 'NONE', #5777, #3764, #12975 ) ;
#6849 = FACE_BOUND ( 'NONE', #11302, .T. ) ;
#6850 = CARTESIAN_POINT ( 'NONE',  ( -243.4994605518340620, -7.743136872103179691, 9.167522614742150466 ) ) ;
#6851 = DIRECTION ( 'NONE',  ( 0.000000000000000000, 0.000000000000000000, -1.000000000000000000 ) ) ;
#6852 = CARTESIAN_POINT ( 'NONE',  ( -239.0755113754114802, 1.313873757884649329, -11.92786187209476623 ) ) ;
#6853 = ITEM_DEFINED_TRANSFORMATION ( 'NONE', 'NONE', #7827,  #805 ) ;
#6854 = APPLICATION_CONTEXT ( 'automotive_design' ) ;
#6855 = ORIENTED_EDGE ( 'NONE', *, *, #1252, .T. ) ;
#6856 = DIRECTION ( 'NONE',  ( 0.000000000000000000, -0.8757116489157734662, -0.4828344519120573719 ) ) ;
#6857 = ORIENTED_EDGE ( 'NONE', *, *, #521, .F. ) ;
#6858 = EDGE_CURVE ( 'NONE', #10530, #2838, #3279, .T. ) ;
#6859 = EDGE_CURVE ( 'NONE', #7354, #2094, #11389, .T. ) ;
#6860 = EDGE_LOOP ( 'NONE', ( #4944, #1839 ) ) ;
#6861 = CARTESIAN_POINT ( 'NONE',  ( -249.6759349623802962, -11.17873215480379478, -3.619182053975217972 ) ) ;
#6862 = EDGE_LOOP ( 'NONE', ( #2308, #2106, #11565, #8569, #3175, #11445, #6534, #7830, #2614, #2458, #10225, #12209 ) ) ;
#6863 = CARTESIAN_POINT ( 'NONE',  ( 130.9697226060475259, 20.55460285142580545, -226.7975291077671329 ) ) ;
#6864 = DIRECTION ( 'NONE',  ( 0.000000000000000000, 0.000000000000000000, 1.000000000000000000 ) ) ;
#6865 = DIRECTION ( 'NONE',  ( 0.000000000000000000, 1.000000000000000000, 0.000000000000000000 ) ) ;
#6866 = DIRECTION ( 'NONE',  ( -0.5469441386039890496, 0.000000000000000000, 0.8371691043312220470 ) ) ;
#6867 = CARTESIAN_POINT ( 'NONE',  ( -240.3908911752174333, 3.583360156783556683, 11.45287536843322052 ) ) ;
#6868 = EDGE_CURVE ( 'NONE', #4826, #3738, #2444, .T. ) ;
#6869 = CARTESIAN_POINT ( 'NONE',  ( -248.0831933713610056, 9.830508068705238856, -6.436117704883929314 ) ) ;
#6870 = CARTESIAN_POINT ( 'NONE',  ( -10.83189848055820725, -138.4705547276867321, -40.42519547187239226 ) ) ;
#6871 = CARTESIAN_POINT ( 'NONE',  ( 229.9849648984647956, 2.315196995243969713, 2.634778663479427241 ) ) ;
#6872 = PRODUCT_DEFINITION_SHAPE ( 'NONE', 'NONE',  #13142 ) ;
#6873 = CARTESIAN_POINT ( 'NONE',  ( -249.2901971947193829, 10.52637179445783566, -5.220957665098429956 ) ) ;
#6874 = CIRCLE ( 'NONE', #2801, 6.500000000000026645 ) ;
#6875 = CARTESIAN_POINT ( 'NONE',  ( -229.9813818884356067, -11.63826747946651530, -2.948217368118681403 ) ) ;
#6876 =( GEOMETRIC_REPRESENTATION_CONTEXT ( 3 ) GLOBAL_UNCERTAINTY_ASSIGNED_CONTEXT ( ( #1854 ) ) GLOBAL_UNIT_ASSIGNED_CONTEXT ( ( #3560, #3425, #11441 ) ) REPRESENTATION_CONTEXT ( 'NONE', 'WORKASPACE' ) );
#6877 = ORIENTED_EDGE ( 'NONE', *, *, #6227, .F. ) ;
#6878 = ORIENTED_EDGE ( 'NONE', *, *, #5568, .F. ) ;
#6879 = CARTESIAN_POINT ( 'NONE',  ( 3.070225547948624535E-14, 19.00000000000000000, -250.7029414592220178 ) ) ;
#6880 = DIRECTION ( 'NONE',  ( 0.000000000000000000, -1.000000000000000000, 0.000000000000000000 ) ) ;
#6882 = EDGE_CURVE ( 'NONE', #1281, #3345, #6202, .T. ) ;
#6881 = AXIS2_PLACEMENT_3D ( 'NONE', #3542, #11692, #2545 ) ;
#6883 = CARTESIAN_POINT ( 'NONE',  ( 234.8993005740659044, 20.55460285055905700, 115.8123742914903289 ) ) ;
#6884 = AXIS2_PLACEMENT_3D ( 'NONE', #10443, #6449, #12449 ) ;
#6885 = EDGE_CURVE ( 'NONE', #2835, #11841, #4350, .T. ) ;
#6886 = DIRECTION ( 'NONE',  ( 0.000000000000000000, 0.000000000000000000, 1.000000000000000000 ) ) ;
#6887 = DIRECTION ( 'NONE',  ( -0.1736481776669207000, 0.000000000000000000, -0.9848077530122097967 ) ) ;
#6888 = CIRCLE ( 'NONE', #8387, 6.500000000000005329 ) ;
#6889 = CIRCLE ( 'NONE', #12001, 2.000000000000000444 ) ;
#6890 = CARTESIAN_POINT ( 'NONE',  ( 239.7985776503625175, 1.848645179571945185, -2.971954070985139751 ) ) ;
#6891 = CONICAL_SURFACE ( 'NONE', #1781, 5.100000000000003197, 0.7853981633974461696 ) ;
#6892 = ORIENTED_EDGE ( 'NONE', *, *, #12723, .F. ) ;
#6893 = DIRECTION ( 'NONE',  ( 0.000000000000000000, 1.000000000000000000, 0.000000000000000000 ) ) ;
#6894 = UNCERTAINTY_MEASURE_WITH_UNIT (LENGTH_MEASURE( 1.000000000000000082E-05 ), #4560, 'distance_accuracy_value', 'NONE');
#6895 = FACE_OUTER_BOUND ( 'NONE', #3866, .T. ) ;
#6896 = ORIENTED_EDGE ( 'NONE', *, *, #1329, .T. ) ;
#6897 = ORIENTED_EDGE ( 'NONE', *, *, #9987, .T. ) ;
#6898 = CIRCLE ( 'NONE', #1575, 2.000000000000001776 ) ;
#6899 = DIRECTION ( 'NONE',  ( 0.000000000000000000, 1.000000000000000000, 0.000000000000000000 ) ) ;
#6900 = ORIENTED_EDGE ( 'NONE', *, *, #6492, .T. ) ;
#6901 = DIRECTION ( 'NONE',  ( 0.000000000000000000, -0.01970892327970899874, -0.9998057603070481525 ) ) ;
#6902 = CARTESIAN_POINT ( 'NONE',  ( -83.95474316043620888, 20.08915143278693094, 247.2466869562449858 ) ) ;
#6903 = EDGE_CURVE ( 'NONE', #3038, #3688, #6069, .T. ) ;
#6904 = CARTESIAN_POINT ( 'NONE',  ( 189.4681260268079086, -19.00000000000000000, 229.3645116836727311 ) ) ;
#6905 =( NAMED_UNIT ( * ) PLANE_ANGLE_UNIT ( ) SI_UNIT ( $, .RADIAN. ) );
#6906 = CARTESIAN_POINT ( 'NONE',  ( 71.82423009839129691, 19.40000000000000213, -202.4354503650404808 ) ) ;
#6907 = PRODUCT_DEFINITION_SHAPE ( 'NONE', 'NONE',  #13081 ) ;
#6908 = AXIS2_PLACEMENT_3D ( 'NONE', #9624, #4369, #3295 ) ;
#6909 = VERTEX_POINT ( 'NONE', #12333 ) ;
#6910 = CYLINDRICAL_SURFACE ( 'NONE', #7323, 5.099999999999993427 ) ;
#6911 = EDGE_LOOP ( 'NONE', ( #2363, #11749, #3979, #1320, #7411 ) ) ;
#6912 = CARTESIAN_POINT ( 'NONE',  ( -246.2764285610849129, 9.322503224274816702, -7.152604636902116120 ) ) ;
#6913 = VERTEX_POINT ( 'NONE', #2388 ) ;
#6914 = AXIS2_PLACEMENT_3D ( 'NONE', #9390, #6460, #4314 ) ;
#6915 = CIRCLE ( 'NONE', #8831, 5.500000000000005329 ) ;
#6916 = CARTESIAN_POINT ( 'NONE',  ( 0.000000000000000000, 18.00000000000000000, 208.0000000000000000 ) ) ;
#6917 = DIRECTION ( 'NONE',  ( 0.000000000000000000, 1.000000000000000000, 0.000000000000000000 ) ) ;
#6918 = CARTESIAN_POINT ( 'NONE',  ( -249.7604317440028296, -11.15122115098357014, 4.588451767773564782 ) ) ;
#6919 = FACE_OUTER_BOUND ( 'NONE', #436, .T. ) ;
#6920 = FACE_BOUND ( 'NONE', #108, .T. ) ;
#6921 = CARTESIAN_POINT ( 'NONE',  ( -242.7490684265873711, -7.085544781346608367, 9.685620095554028808 ) ) ;
#6922 = CARTESIAN_POINT ( 'NONE',  ( -158.8368823490021953, 20.79694577634646535, -206.9952515782969726 ) ) ;
#6923 = UNCERTAINTY_MEASURE_WITH_UNIT (LENGTH_MEASURE( 1.000000000000000082E-05 ), #2321, 'distance_accuracy_value', 'NONE');
#6924 = VERTEX_POINT ( 'NONE', #4258 ) ;
#6925 = CARTESIAN_POINT ( 'NONE',  ( 227.3999999999999773, 0.1024105694487990881, 5.195143123655512341 ) ) ;
#6926 = ORIENTED_EDGE ( 'NONE', *, *, #3786, .T. ) ;
#6927 = EDGE_LOOP ( 'NONE', ( #12379, #4149, #3217, #9021 ) ) ;
#6928 = CARTESIAN_POINT ( 'NONE',  ( -249.7834965323052074, -11.60135170610416822, -1.863160430645350418 ) ) ;
#6929 = ORIENTED_EDGE ( 'NONE', *, *, #3382, .T. ) ;
#6930 = CARTESIAN_POINT ( 'NONE',  ( 84.20717312453921011, 20.55460285117019126, -247.9906035365278001 ) ) ;
#6931 = CARTESIAN_POINT ( 'NONE',  ( -249.7118339206215012, 9.997999799959989886, -6.636264009214830395 ) ) ;
#6932 = CARTESIAN_POINT ( 'NONE',  ( 71.82423009839129691, 30.00000000000000000, -190.8354503650404865 ) ) ;
#6933 = CARTESIAN_POINT ( 'NONE',  ( -31.19222893191935242, -19.00000000000000000, 286.4438302234617595 ) ) ;
#6934 = VECTOR ( 'NONE', #3643, 1000.000000000000114 ) ;
#6935 = AXIS2_PLACEMENT_3D ( 'NONE', #7300, #12240, #12297 ) ;
#6936 = EDGE_CURVE ( 'NONE', #808, #3020, #3717, .T. ) ;
#6937 = DIRECTION ( 'NONE',  ( 0.000000000000000000, 1.000000000000000000, 0.000000000000000000 ) ) ;
#6938 = EDGE_CURVE ( 'NONE', #9902, #644, #1811, .T. ) ;
#6939 = CARTESIAN_POINT ( 'NONE',  ( 0.000000000000000000, 19.00000000000000000, 0.000000000000000000 ) ) ;
#6940 = CARTESIAN_POINT ( 'NONE',  ( 7.267391899530378119, -138.4705547276867321, -41.21542755584190587 ) ) ;
#6941 = LINE ( 'NONE', #4994, #10311 ) ;
#6942 = ITEM_DEFINED_TRANSFORMATION ( 'NONE', 'NONE', #2984,  #805 ) ;
#6943 = CIRCLE ( 'NONE', #1198, 246.0000000000000000 ) ;
#6944 = LINE ( 'NONE', #10802, #8778 ) ;
#6945 = ORIENTED_EDGE ( 'NONE', *, *, #12004, .F. ) ;
#6946 = EDGE_LOOP ( 'NONE', ( #9087, #629, #11019, #5901 ) ) ;
#6947 = DIRECTION ( 'NONE',  ( 1.224646799147349509E-16, 0.000000000000000000, -1.000000000000000000 ) ) ;
#6948 = CARTESIAN_POINT ( 'NONE',  ( 153.9282213272189495, -30.00000000000000000, 245.7765299597151341 ) ) ;
#6949 = CARTESIAN_POINT ( 'NONE',  ( 34.13493237066314379, 20.79694577651677889, -259.0935598596149703 ) ) ;
#6950 = CARTESIAN_POINT ( 'NONE',  ( 3.012631125902489062E-14, 21.99999999999995381, 246.0000000000000000 ) ) ;
#6951 = CARTESIAN_POINT ( 'NONE',  ( 0.000000000000000000, 0.000000000000000000, 0.000000000000000000 ) ) ;
#6952 = CARTESIAN_POINT ( 'NONE',  ( -245.2595250088976115, -8.869312996839244789, 7.707186824084115706 ) ) ;
#6953 = VERTEX_POINT ( 'NONE', #2701 ) ;
#6954 = CARTESIAN_POINT ( 'NONE',  ( 122.2593324768334071, 29.00000000000000000, -162.7755348299894820 ) ) ;
#6955 = CARTESIAN_POINT ( 'NONE',  ( -239.0946434582524489, -1.343932714108268645, 11.92448114257838121 ) ) ;
#6956 = ORIENTED_EDGE ( 'NONE', *, *, #5890, .T. ) ;
#6957 = VERTEX_POINT ( 'NONE', #6597 ) ;
#6958 = EDGE_CURVE ( 'NONE', #7179, #1648, #325, .T. ) ;
#6959 = EDGE_CURVE ( 'NONE', #13033, #4811, #4990, .T. ) ;
#6960 = FACE_OUTER_BOUND ( 'NONE', #184, .T. ) ;
#6961 = ORIENTED_EDGE ( 'NONE', *, *, #8372, .F. ) ;
#6962 =( REPRESENTATION_RELATIONSHIP ('NONE','NONE', #12019, #5191 ) REPRESENTATION_RELATIONSHIP_WITH_TRANSFORMATION ( #10002 )SHAPE_REPRESENTATION_RELATIONSHIP( ) );
#6963 = CARTESIAN_POINT ( 'NONE',  ( 0.000000000000000000, 0.000000000000000000, 0.000000000000000000 ) ) ;
#6964 = CARTESIAN_POINT ( 'NONE',  ( -130.8783844633512956, 19.96883746151126360, 226.6392846543344035 ) ) ;
#6965 = CARTESIAN_POINT ( 'NONE',  ( -239.4471451945621254, -1.776586343123336853, -11.86775802751313869 ) ) ;
#6966 = FACE_OUTER_BOUND ( 'NONE', #12715, .T. ) ;
#6967 = ORIENTED_EDGE ( 'NONE', *, *, #1329, .F. ) ;
#6968 = DIRECTION ( 'NONE',  ( 0.000000000000000000, -0.9998057603070481525, 0.01970892327970912364 ) ) ;
#6969 = EDGE_LOOP ( 'NONE', ( #9617, #3473, #3536, #6508 ) ) ;
#6970 = CARTESIAN_POINT ( 'NONE',  ( -245.1951802367414075, 8.836085396024165206, -7.745290894946786686 ) ) ;
#6971 = ORIENTED_EDGE ( 'NONE', *, *, #119, .T. ) ;
#6972 = AXIS2_PLACEMENT_3D ( 'NONE', #11928, #5868, #6866 ) ;
#6973 = EDGE_CURVE ( 'NONE', #237, #12419, #12453, .T. ) ;
#6974 = DIRECTION ( 'NONE',  ( 0.000000000000000000, 0.000000000000000000, 1.000000000000000000 ) ) ;
#6975 = CARTESIAN_POINT ( 'NONE',  ( 0.000000000000000000, 18.00000000000000000, -230.0000000000000000 ) ) ;
#6976 = CARTESIAN_POINT ( 'NONE',  ( 239.0147185140285728, 0.4456008733042243208, 3.471580854525857074 ) ) ;
#6977 = DIRECTION ( 'NONE',  ( 0.000000000000000000, 0.000000000000000000, 1.000000000000000000 ) ) ;
#6978 = EDGE_CURVE ( 'NONE', #4030, #1172, #8411, .T. ) ;
#6979 = DIRECTION ( 'NONE',  ( 0.000000000000000000, 0.000000000000000000, 1.000000000000000000 ) ) ;
#6980 = PRODUCT_DEFINITION_SHAPE ( 'NONE', 'NONE',  #13103 ) ;
#6981 = CARTESIAN_POINT ( 'NONE',  ( -242.3889174895368228, -6.718220498460057755, 9.943174756676034676 ) ) ;
#6982 = CIRCLE ( 'NONE', #5917, 248.7999999999999829 ) ;
#6983 = CARTESIAN_POINT ( 'NONE',  ( -212.0849693193236760, 20.79694577634646535, -151.9741924115234895 ) ) ;
#6984 = ORIENTED_EDGE ( 'NONE', *, *, #3117, .F. ) ;
#6985 = CARTESIAN_POINT ( 'NONE',  ( -238.7146408298738720, -0.1451103193397513536, -11.74918806529056603 ) ) ;
#6986 = EDGE_LOOP ( 'NONE', ( #8437, #9052, #5878, #3450 ) ) ;
#6987 = VERTEX_POINT ( 'NONE', #4513 ) ;
#6988 = CARTESIAN_POINT ( 'NONE',  ( -249.2689385757789466, -10.50219330951161467, -5.269387968823961543 ) ) ;
#6989 = EDGE_LOOP ( 'NONE', ( #3284, #11899, #4607, #8645 ) ) ;
#6990 = AXIS2_PLACEMENT_3D ( 'NONE', #12146, #11413, #4203 ) ;
#6991 = CARTESIAN_POINT ( 'NONE',  ( 172.6991790965608971, 20.55460285089974093, 196.8887528236631965 ) ) ;
#6992 = CARTESIAN_POINT ( 'NONE',  ( -247.6787047776036559, 9.753293420611971243, -6.991498264524891759 ) ) ;
#6993 = DIRECTION ( 'NONE',  ( -0.000000000000000000, -1.000000000000000000, 0.000000000000000000 ) ) ;
#6994 = CARTESIAN_POINT ( 'NONE',  ( 0.000000000000000000, -2.772967769359314882, 0.000000000000000000 ) ) ;
#6995 = CARTESIAN_POINT ( 'NONE',  ( -243.4327047837443274, 7.689587473932653516, 9.212521827026886712 ) ) ;
#6996 = CARTESIAN_POINT ( 'NONE',  ( 0.000000000000000000, 30.00000000000000000, 0.000000000000000000 ) ) ;
#6997 = DIRECTION ( 'NONE',  ( -0.4999999999999919509, 0.000000000000000000, -0.8660254037844432595 ) ) ;
#6998 = CONICAL_SURFACE ( 'NONE', #10397, 6.500000000000005329, 0.7853981633974476129 ) ;
#6999 = CARTESIAN_POINT ( 'NONE',  ( -230.0000069428143377, -11.75013590190525115, 0.3790685594532250957 ) ) ;
#7000 = CONTEXT_DEPENDENT_SHAPE_REPRESENTATION ( #7888, #7197 ) ;
#7001 = CIRCLE ( 'NONE', #6587, 6.500000000000005329 ) ;
#7002 = AXIS2_PLACEMENT_3D ( 'NONE', #7623, #11568, #5556 ) ;
#7003 = VECTOR ( 'NONE', #2023, 1000.000000000000000 ) ;
#7004 = DIRECTION ( 'NONE',  ( 0.6368676505102716101, 0.000000000000000000, 0.7709731485165527420 ) ) ;
#7005 = ORIENTED_EDGE ( 'NONE', *, *, #6882, .T. ) ;
#7006 = AXIS2_PLACEMENT_3D ( 'NONE', #1729, #1530, #9856 ) ;
#7007 = ORIENTED_EDGE ( 'NONE', *, *, #3335, .T. ) ;
#7008 = CONICAL_SURFACE ( 'NONE', #623, 5.500000000000005329, 0.7853981633974461696 ) ;
#7009 = EDGE_CURVE ( 'NONE', #5207, #13031, #10955, .T. ) ;
#7010 = CARTESIAN_POINT ( 'NONE',  ( 229.9000000000000057, -3.999223041228192610, 0.07883569311883648068 ) ) ;
#7011 = DIRECTION ( 'NONE',  ( 0.000000000000000000, 1.000000000000000000, 0.000000000000000000 ) ) ;
#7012 = FACE_OUTER_BOUND ( 'NONE', #4711, .T. ) ;
#7013 = DIRECTION ( 'NONE',  ( 0.000000000000000000, 0.000000000000000000, 1.000000000000000000 ) ) ;
#7014 = CARTESIAN_POINT ( 'NONE',  ( -27.68945685411286561, -30.00000000000000000, 290.6841825403027997 ) ) ;
#7015 = AXIS2_PLACEMENT_3D ( 'NONE', #7111, #10431, #4233 ) ;
#7016 = CARTESIAN_POINT ( 'NONE',  ( 0.000000000000000000, 0.000000000000000000, 0.000000000000000000 ) ) ;
#7017 = CARTESIAN_POINT ( 'NONE',  ( -197.8197553893909912, 18.00000000000000000, 70.77553482999131518 ) ) ;
#7018 = ORIENTED_EDGE ( 'NONE', *, *, #4405, .F. ) ;
#7019 = LINE ( 'NONE', #7086, #4239 ) ;
#7020 = AXIS2_PLACEMENT_3D ( 'NONE', #5003, #3937, #634 ) ;
#7021 = CARTESIAN_POINT ( 'NONE',  ( -238.8648708971568624, -0.8933728624606902535, 11.96676141197713505 ) ) ;
#7022 = ORIENTED_EDGE ( 'NONE', *, *, #11779, .F. ) ;
#7023 = ORIENTED_EDGE ( 'NONE', *, *, #8203, .F. ) ;
#7024 = EDGE_CURVE ( 'NONE', #1244, #1953, #10100, .T. ) ;
#7025 = AXIS2_PLACEMENT_3D ( 'NONE', #9574, #1447, #10710 ) ;
#7026 = CARTESIAN_POINT ( 'NONE',  ( 157.1762463448213225, -19.40000000000000213, 249.7084930171495500 ) ) ;
#7027 = FACE_OUTER_BOUND ( 'NONE', #10372, .T. ) ;
#7028 = CARTESIAN_POINT ( 'NONE',  ( -249.2564709990199958, 10.48830713231970790, 5.296988133095193341 ) ) ;
#7029 = CARTESIAN_POINT ( 'NONE',  ( 258.8746690706134927, 20.08915143329815933, 34.10614053548034974 ) ) ;
#7030 = CIRCLE ( 'NONE', #5263, 230.0000000000000000 ) ;
#7031 = CARTESIAN_POINT ( 'NONE',  ( -238.7551951684716869, -0.5376686924967483128, -11.98842779547521609 ) ) ;
#7032 =( NAMED_UNIT ( * ) PLANE_ANGLE_UNIT ( ) SI_UNIT ( $, .RADIAN. ) );
#7033 = CARTESIAN_POINT ( 'NONE',  ( -242.0448478360703177, 6.321212805588819705, 9.907269458070054213 ) ) ;
#7034 = EDGE_CURVE ( 'NONE', #12935, #11832, #10651, .T. ) ;
#7035 = VERTEX_POINT ( 'NONE', #8786 ) ;
#7036 = CARTESIAN_POINT ( 'NONE',  ( -239.2643540567006539, -1.566629693467802786, 11.64555736025064903 ) ) ;
#7037 = ORIENTED_EDGE ( 'NONE', *, *, #7552, .F. ) ;
#7038 = VECTOR ( 'NONE', #6614, 1000.000000000000000 ) ;
#7039 = CARTESIAN_POINT ( 'NONE',  ( -244.9693137024618750, 8.715706973424389048, -7.881056914057721130 ) ) ;
#7040 = VERTEX_POINT ( 'NONE', #11988 ) ;
#7041 = DIRECTION ( 'NONE',  ( 0.000000000000000000, 1.000000000000000000, 0.000000000000000000 ) ) ;
#7042 = AXIS2_PLACEMENT_3D ( 'NONE', #6545, #1471, #10540 ) ;
#7043 = CARTESIAN_POINT ( 'NONE',  ( 71.82423009839129691, 28.60000000000000142, -202.4354503650404808 ) ) ;
#7044 = DIRECTION ( 'NONE',  ( 0.000000000000000000, -1.000000000000000000, 0.000000000000000000 ) ) ;
#7045 = DIRECTION ( 'NONE',  ( -0.7071067811865490160, -0.7069694329824840473, 0.01393631330096761593 ) ) ;
#7046 = CARTESIAN_POINT ( 'NONE',  ( -115.3046144132251527, 20.08915143297737060, -233.8077470125392949 ) ) ;
#7047 = PRESENTATION_STYLE_ASSIGNMENT (( #2967 ) ) ;
#7048 = EDGE_CURVE ( 'NONE', #58, #3502, #6915, .T. ) ;
#7049 = EDGE_CURVE ( 'NONE', #6308, #7991, #788, .T. ) ;
#7050 = CARTESIAN_POINT ( 'NONE',  ( -239.3393815581031561, 1.669038143830544607, -11.88372659505663798 ) ) ;
#7051 = ORIENTED_EDGE ( 'NONE', *, *, #6319, .F. ) ;
#7052 = LINE ( 'NONE', #12181, #8802 ) ;
#7053 = CIRCLE ( 'NONE', #7362, 6.500000000000005329 ) ;
#7054 = ORIENTED_EDGE ( 'NONE', *, *, #12232, .F. ) ;
#7055 = CARTESIAN_POINT ( 'NONE',  ( -246.2633612345466645, -9.321506464518613200, -7.557087660178679833 ) ) ;
#7056 = EDGE_CURVE ( 'NONE', #12848, #2492, #2296, .T. ) ;
#7057 = CARTESIAN_POINT ( 'NONE',  ( 17.05322212017823347, 20.08915143297737060, -260.1353576186481860 ) ) ;
#7058 = EDGE_LOOP ( 'NONE', ( #5674, #2473 ) ) ;
#7059 = CIRCLE ( 'NONE', #1311, 2.749999999999999556 ) ;
#7060 = CARTESIAN_POINT ( 'NONE',  ( -259.0935598604214647, 20.79694577620453799, 34.13493237032840000 ) ) ;
#7061 = DIRECTION ( 'NONE',  ( 0.6368676505102737195, 0.000000000000000000, 0.7709731485165509657 ) ) ;
#7062 = PLANE ( 'NONE',  #9976 ) ;
#7063 = CARTESIAN_POINT ( 'NONE',  ( -241.4114469337881133, -5.479936497601446632, -10.39393372303794294 ) ) ;
#7064 = CIRCLE ( 'NONE', #11625, 5.499999999999986677 ) ;
#7065 = CARTESIAN_POINT ( 'NONE',  ( -247.2298618829602503, 9.638957510244241078, 7.147826786188287151 ) ) ;
#7066 = EDGE_CURVE ( 'NONE', #11098, #12785, #3776, .T. ) ;
#7067 = DIRECTION ( 'NONE',  ( -0.000000000000000000, -1.000000000000000000, 0.000000000000000000 ) ) ;
#7068 = CARTESIAN_POINT ( 'NONE',  ( 37.93010648591150158, -138.4705547276867321, 17.68709912901561765 ) ) ;
#7069 = DIRECTION ( 'NONE',  ( 0.5469441386039890496, 0.000000000000000000, -0.8371691043312220470 ) ) ;
#7070 = PLANE ( 'NONE',  #2174 ) ;
#7071 = ORIENTED_EDGE ( 'NONE', *, *, #5542, .F. ) ;
#7072 = VERTEX_POINT ( 'NONE', #3913 ) ;
#7073 = VECTOR ( 'NONE', #544, 1000.000000000000000 ) ;
#7074 = DIRECTION ( 'NONE',  ( 0.7071067811865480168, 0.7069694329824850465, -0.01393631330096763501 ) ) ;
#7075 = CARTESIAN_POINT ( 'NONE',  ( 0.000000000000000000, -1.848645179579245124, 239.8169934640528993 ) ) ;
#7076 = CARTESIAN_POINT ( 'NONE',  ( 238.9743710625051278, -0.08886714779590801361, -3.499996468587203147 ) ) ;
#7077 = VECTOR ( 'NONE', #7139, 999.9999999999998863 ) ;
#7078 = CARTESIAN_POINT ( 'NONE',  ( -210.0000000000000000, 18.00000000000000000, 6.500000000000007994 ) ) ;
#7079 = DIRECTION ( 'NONE',  ( 0.000000000000000000, -1.000000000000000000, 0.000000000000000000 ) ) ;
#7080 = CARTESIAN_POINT ( 'NONE',  ( 0.000000000000000000, 0.000000000000000000, 0.000000000000000000 ) ) ;
#7081 = AXIS2_PLACEMENT_3D ( 'NONE', #2282, #4216, #11560 ) ;
#7082 = CARTESIAN_POINT ( 'NONE',  ( -244.2253259529525167, -8.263305842909222321, 8.353459642369911009 ) ) ;
#7083 = ITEM_DEFINED_TRANSFORMATION ( 'NONE', 'NONE', #6146,  #805 ) ;
#7084 = ORIENTED_EDGE ( 'NONE', *, *, #7989, .T. ) ;
#7085 = AXIS2_PLACEMENT_3D ( 'NONE', #509, #12695, #7629 ) ;
#7086 = CARTESIAN_POINT ( 'NONE',  ( 122.2593324768334071, 30.00000000000000000, -161.7755348299894820 ) ) ;
#7087 = CARTESIAN_POINT ( 'NONE',  ( 229.9933911495604377, -3.037488298063726777, 1.754034819793648836 ) ) ;
#7088 = EDGE_LOOP ( 'NONE', ( #12480, #4144, #6304, #1761 ) ) ;
#7089 = ORIENTED_EDGE ( 'NONE', *, *, #5583, .F. ) ;
#7090 = DIRECTION ( 'NONE',  ( -0.000000000000000000, -1.000000000000000000, 0.000000000000000000 ) ) ;
#7091 = FACE_OUTER_BOUND ( 'NONE', #4896, .T. ) ;
#7092 = PRODUCT_DEFINITION_SHAPE ( 'NONE', 'NONE',  #13148 ) ;
#7093 = FACE_OUTER_BOUND ( 'NONE', #2740, .T. ) ;
#7094 = AXIS2_PLACEMENT_3D ( 'NONE', #11311, #12573, #10699 ) ;
#7095 = CARTESIAN_POINT ( 'NONE',  ( -252.8031682270705289, 19.96883745940372279, 67.71318189758537187 ) ) ;
#7096 = CARTESIAN_POINT ( 'NONE',  ( -239.1634599900678495, -1.446074388866761540, -11.91252809098397236 ) ) ;
#7097 = DIRECTION ( 'NONE',  ( 0.000000000000000000, 0.000000000000000000, 1.000000000000000000 ) ) ;
#7098 = CARTESIAN_POINT ( 'NONE',  ( -244.3371393072379760, 8.336835368989806483, 8.280174500310611307 ) ) ;
#7099 = EDGE_CURVE ( 'NONE', #6838, #3954, #751, .T. ) ;
#7100 = EDGE_CURVE ( 'NONE', #11817, #2751, #7052, .T. ) ;
#7101 = VERTEX_POINT ( 'NONE', #11047 ) ;
#7102 = CARTESIAN_POINT ( 'NONE',  ( -239.3739003381174939, -1.702175412253983611, 11.62699861431983273 ) ) ;
#7103 = CIRCLE ( 'NONE', #8173, 6.500000000000005329 ) ;
#7104 = CIRCLE ( 'NONE', #3044, 6.500000000000005329 ) ;
#7105 = EDGE_LOOP ( 'NONE', ( #11498, #9847 ) ) ;
#7106 = VECTOR ( 'NONE', #6562, 1000.000000000000000 ) ;
#7107 = DIRECTION ( 'NONE',  ( 0.000000000000000000, -1.000000000000000000, 0.000000000000000000 ) ) ;
#7108 = ORIENTED_EDGE ( 'NONE', *, *, #11196, .T. ) ;
#7109 =( REPRESENTATION_RELATIONSHIP ('NONE','NONE', #12019, #182 ) REPRESENTATION_RELATIONSHIP_WITH_TRANSFORMATION ( #4110 )SHAPE_REPRESENTATION_RELATIONSHIP( ) );
#7110 = CARTESIAN_POINT ( 'NONE',  ( -289.8128292627096130, -28.60000000000000142, 10.41748504886635907 ) ) ;
#7111 = CARTESIAN_POINT ( 'NONE',  ( 0.000000000000000000, 21.50000000000000000, 0.000000000000000000 ) ) ;
#7112 = CARTESIAN_POINT ( 'NONE',  ( 0.000000000000000000, 0.000000000000000000, 0.000000000000000000 ) ) ;
#7113 = CARTESIAN_POINT ( 'NONE',  ( -24.18668477630637526, -30.00000000000000000, 294.9245348571438967 ) ) ;
#7114 = CIRCLE ( 'NONE', #12638, 250.3823410207189966 ) ;
#7115 = DIRECTION ( 'NONE',  ( 0.4503334343941555740, 0.7071067811865490160, 0.5451603414287971017 ) ) ;
#7116 = CARTESIAN_POINT ( 'NONE',  ( 227.3999999999999773, 4.550331206106116078, 2.508881407069060376 ) ) ;
#7117 = AXIS2_PLACEMENT_3D ( 'NONE', #3588, #2586, #10789 ) ;
#7118 = CARTESIAN_POINT ( 'NONE',  ( -257.4287020129719963, 20.79694577634646535, -42.50473797389778241 ) ) ;
#7119 = EDGE_LOOP ( 'NONE', ( #9037, #8359, #5193, #10780 ) ) ;
#7120 = CARTESIAN_POINT ( 'NONE',  ( -239.2060324344808748, -1.486384979126868844, -11.65560575368058949 ) ) ;
#7121 = VERTEX_POINT ( 'NONE', #6114 ) ;
#7122 = CARTESIAN_POINT ( 'NONE',  ( -249.7981860219790633, 11.73141662443953059, 0.7273454842090188999 ) ) ;
#7123 = LINE ( 'NONE', #11181, #6196 ) ;
#7124 = VECTOR ( 'NONE', #6773, 1000.000000000000000 ) ;
#7125 = TOROIDAL_SURFACE ( 'NONE', #3066, 261.5294117647060261, 2.000000000000000000 ) ;
#7126 = CARTESIAN_POINT ( 'NONE',  ( -249.7367190362209897, -11.37209550593751572, 2.959943712984164144 ) ) ;
#7127 = ORIENTED_EDGE ( 'NONE', *, *, #10434, .T. ) ;
#7128 = ADVANCED_FACE ( 'NONE', ( #5990 ), #983, .T. ) ;
#7129 = CARTESIAN_POINT ( 'NONE',  ( -84.02568524183371323, 20.79694577604410100, 247.4557548106605225 ) ) ;
#7130 = EDGE_CURVE ( 'NONE', #2425, #3848, #7313, .T. ) ;
#7131 = CARTESIAN_POINT ( 'NONE',  ( -247.9991062033159039, 9.816924796666317121, -6.901310522998599595 ) ) ;
#7132 = DIRECTION ( 'NONE',  ( -1.000000000000000000, 0.000000000000000000, 0.000000000000000000 ) ) ;
#7133 = CARTESIAN_POINT ( 'NONE',  ( -246.8900737883909358, -9.535158805240152802, -6.866190024035137007 ) ) ;
#7134 = CARTESIAN_POINT ( 'NONE',  ( -249.7118339206215012, 9.997999799959989886, 6.636264009214830395 ) ) ;
#7135 = AXIS2_PLACEMENT_3D ( 'NONE', #4060, #8139, #12202 ) ;
#7136 = DIRECTION ( 'NONE',  ( -1.000000000000000000, 0.000000000000000000, 0.000000000000000000 ) ) ;
#7137 = CARTESIAN_POINT ( 'NONE',  ( 26.90145978217088185, -138.4705547276867321, 32.05991134143159371 ) ) ;
#7138 = CARTESIAN_POINT ( 'NONE',  ( -229.9999859999076932, -11.74972595562163136, -0.7707053339805227665 ) ) ;
#7139 = DIRECTION ( 'NONE',  ( 0.000000000000000000, -0.7071067811865771047, -0.7071067811865180408 ) ) ;
#7140 = ORIENTED_EDGE ( 'NONE', *, *, #11862, .T. ) ;
#7141 = ORIENTED_EDGE ( 'NONE', *, *, #12585, .F. ) ;
#7142 = CIRCLE ( 'NONE', #1602, 3.000000000000002665 ) ;
#7143 = CARTESIAN_POINT ( 'NONE',  ( 260.5542428351129729, 20.08915143297737416, -17.05314194230804858 ) ) ;
#7144 = ADVANCED_FACE ( 'NONE', ( #9112 ), #9050, .F. ) ;
#7145 = DIRECTION ( 'NONE',  ( 0.000000000000000000, 1.000000000000000000, 0.000000000000000000 ) ) ;
#7146 = DIRECTION ( 'NONE',  ( 0.000000000000000000, 0.000000000000000000, 1.000000000000000000 ) ) ;
#7147 = CARTESIAN_POINT ( 'NONE',  ( 247.4557548098379982, 20.79694577642534270, 84.02568524150230189 ) ) ;
#7148 = EDGE_CURVE ( 'NONE', #8308, #10559, #11240, .T. ) ;
#7149 = DIRECTION ( 'NONE',  ( 0.6368676505102706109, 0.000000000000000000, 0.7709731485165535192 ) ) ;
#7150 = CARTESIAN_POINT ( 'NONE',  ( -3.647576077975068998, -138.4705547276867321, 41.69198534955603463 ) ) ;
#7151 = CARTESIAN_POINT ( 'NONE',  ( -240.4180123854748672, -3.650278635874803168, 11.17777342477751645 ) ) ;
#7152 = TOROIDAL_SURFACE ( 'NONE', #4166, 6.053020646647509828, 3.153020646647509917 ) ;
#7153 = ITEM_DEFINED_TRANSFORMATION ( 'NONE', 'NONE', #2358,  #805 ) ;
#7154 = ORIENTED_EDGE ( 'NONE', *, *, #11353, .T. ) ;
#7155 = CARTESIAN_POINT ( 'NONE',  ( 3.059167704270088292E-14, -11.79660968244690089, -249.7999999999999829 ) ) ;
#7156 = DIRECTION ( 'NONE',  ( 0.000000000000000000, 0.000000000000000000, -1.000000000000000000 ) ) ;
#7157 = ORIENTED_EDGE ( 'NONE', *, *, #2273, .T. ) ;
#7158 = ORIENTED_EDGE ( 'NONE', *, *, #7196, .T. ) ;
#7159 = DIRECTION ( 'NONE',  ( 0.000000000000000000, -1.000000000000000000, 0.000000000000000000 ) ) ;
#7160 = FACE_OUTER_BOUND ( 'NONE', #5847, .T. ) ;
#7161 = CARTESIAN_POINT ( 'NONE',  ( -207.6469600138974272, 19.96883745988519365, -159.3024069661565534 ) ) ;
#7162 = DIRECTION ( 'NONE',  ( -0.4503334343941575724, 0.7071067811865460184, -0.5451603414287993221 ) ) ;
#7163 = DIRECTION ( 'NONE',  ( -0.4226182617407002740, 0.000000000000000000, 0.9063077870366496036 ) ) ;
#7164 = CARTESIAN_POINT ( 'NONE',  ( -242.2164292014367675, 6.515245625900396576, 9.778246362781860768 ) ) ;
#7165 = VERTEX_POINT ( 'NONE', #4305 ) ;
#7166 = CARTESIAN_POINT ( 'NONE',  ( 260.7745447061712412, 20.79694577634646890, 8.533827019709855577 ) ) ;
#7167 = ORIENTED_EDGE ( 'NONE', *, *, #7614, .T. ) ;
#7168 = DIRECTION ( 'NONE',  ( 1.000000000000000000, 0.000000000000000000, 0.000000000000000000 ) ) ;
#7169 = EDGE_LOOP ( 'NONE', ( #5487, #5123 ) ) ;
#7170 = EDGE_CURVE ( 'NONE', #6828, #8275, #11358, .T. ) ;
#7171 = DIRECTION ( 'NONE',  ( -0.000000000000000000, -1.000000000000000000, 0.000000000000000000 ) ) ;
#7172 = DIRECTION ( 'NONE',  ( 0.000000000000000000, -1.000000000000000000, 0.000000000000000000 ) ) ;
#7173 = FACE_OUTER_BOUND ( 'NONE', #4312, .T. ) ;
#7174 = CARTESIAN_POINT ( 'NONE',  ( -158.7026972336032316, 20.08915143297737060, -206.8203823583193071 ) ) ;
#7175 = CONICAL_SURFACE ( 'NONE', #1429, 5.499999999999986677, 0.7853981633974461696 ) ;
#7176 = DIRECTION ( 'NONE',  ( -0.000000000000000000, -1.000000000000000000, 0.000000000000000000 ) ) ;
#7177 = CARTESIAN_POINT ( 'NONE',  ( -260.7745447061711843, 20.79694577634646535, -8.533827019710107820 ) ) ;
#7178 = ITEM_DEFINED_TRANSFORMATION ( 'NONE', 'NONE', #12520,  #805 ) ;
#7179 = VERTEX_POINT ( 'NONE', #8388 ) ;
#7180 = FACE_OUTER_BOUND ( 'NONE', #12136, .T. ) ;
#7181 = EDGE_LOOP ( 'NONE', ( #3746, #9800, #6038, #12371 ) ) ;
#7182 = DIRECTION ( 'NONE',  ( 0.000000000000000000, 1.000000000000000000, 0.000000000000000000 ) ) ;
#7183 = CARTESIAN_POINT ( 'NONE',  ( -246.0119047622995936, -9.221725594001977555, -7.678802609089674824 ) ) ;
#7184 = CARTESIAN_POINT ( 'NONE',  ( 27.68945685411497593, -18.00000000000000000, -290.6841825403026291 ) ) ;
#7185 = ORIENTED_EDGE ( 'NONE', *, *, #543, .F. ) ;
#7186 = EDGE_CURVE ( 'NONE', #1872, #7466, #5397, .T. ) ;
#7187 = CARTESIAN_POINT ( 'NONE',  ( 226.3083638779000069, 20.79694577591247295, -130.6873781523096056 ) ) ;
#7188 = CARTESIAN_POINT ( 'NONE',  ( -245.5719560649888251, 9.027896078028849303, -7.905358857574679377 ) ) ;
#7189 = DIRECTION ( 'NONE',  ( 0.6368676505102707219, 0.000000000000000000, 0.7709731485165535192 ) ) ;
#7190 = CARTESIAN_POINT ( 'NONE',  ( -244.2426106971969375, -8.274791045078215390, -8.342083836208937342 ) ) ;
#7191 = AXIS2_PLACEMENT_3D ( 'NONE', #2780, #4651, #1734 ) ;
#7192 = DIRECTION ( 'NONE',  ( -0.2588190451025111916, 0.000000000000000000, -0.9659258262890708657 ) ) ;
#7193 = EDGE_CURVE ( 'NONE', #11448, #12886, #4528, .T. ) ;
#7194 = CARTESIAN_POINT ( 'NONE',  ( 240.6084075703248857, 3.437342788132964788, -0.6677429275107119588 ) ) ;
#7195 = CONTEXT_DEPENDENT_SHAPE_REPRESENTATION ( #6739, #5682 ) ;
#7196 = EDGE_CURVE ( 'NONE', #7625, #1432, #12424, .T. ) ;
#7197 = PRODUCT_DEFINITION_SHAPE ( 'NONE', 'NONE',  #13138 ) ;
#7198 = CARTESIAN_POINT ( 'NONE',  ( 0.000000000000000000, 24.75600756274008063, 0.000000000000000000 ) ) ;
#7199 = ORIENTED_EDGE ( 'NONE', *, *, #8442, .T. ) ;
#7200 = VERTEX_POINT ( 'NONE', #6384 ) ;
#7201 = CARTESIAN_POINT ( 'NONE',  ( 83.95474316029249451, 20.08915143279689630, 247.2466869562504996 ) ) ;
#7202 = DIRECTION ( 'NONE',  ( 1.000000000000000000, 0.000000000000000000, 0.000000000000000000 ) ) ;
#7203 = DIRECTION ( 'NONE',  ( 0.000000000000000000, -1.000000000000000000, 0.000000000000000000 ) ) ;
#7204 = AXIS2_PLACEMENT_3D ( 'NONE', #11356, #6096, #10147 ) ;
#7205 = FACE_OUTER_BOUND ( 'NONE', #3285, .T. ) ;
#7206 = AXIS2_PLACEMENT_3D ( 'NONE', #2305, #12511, #8457 ) ;
#7207 = VECTOR ( 'NONE', #2277, 1000.000000000000000 ) ;
#7208 = CARTESIAN_POINT ( 'NONE',  ( -233.0000000000000000, 0.000000000000000000, 0.000000000000000000 ) ) ;
#7209 = AXIS2_PLACEMENT_3D ( 'NONE', #2861, #7942, #2067 ) ;
#7210 = AXIS2_PLACEMENT_3D ( 'NONE', #4474, #7419, #8559 ) ;
#7211 = DIRECTION ( 'NONE',  ( 0.6368676505102698338, 0.000000000000000000, 0.7709731485165542964 ) ) ;
#7212 = DIRECTION ( 'NONE',  ( 0.1736481776669404620, 0.000000000000000000, -0.9848077530122062440 ) ) ;
#7213 = AXIS2_PLACEMENT_3D ( 'NONE', #9739, #627, #4677 ) ;
#7214 = ADVANCED_FACE ( 'NONE', ( #2107 ), #6681, .F. ) ;
#7215 = CARTESIAN_POINT ( 'NONE',  ( -240.8355308714235719, -4.526241346080312589, 10.84528472031096591 ) ) ;
#7216 =( REPRESENTATION_RELATIONSHIP ('NONE','NONE', #12019, #5191 ) REPRESENTATION_RELATIONSHIP_WITH_TRANSFORMATION ( #1412 )SHAPE_REPRESENTATION_RELATIONSHIP( ) );
#7217 = ITEM_DEFINED_TRANSFORMATION ( 'NONE', 'NONE', #7839,  #805 ) ;
#7218 = ADVANCED_FACE ( 'NONE', ( #12507 ), #5605, .F. ) ;
#7219 = ORIENTED_EDGE ( 'NONE', *, *, #12422, .F. ) ;
#7220 = CARTESIAN_POINT ( 'NONE',  ( 240.4969650423268774, -3.129188642545182475, -1.571450734204370203 ) ) ;
#7221 = DIRECTION ( 'NONE',  ( -0.000000000000000000, -1.000000000000000000, 0.000000000000000000 ) ) ;
#7222 = VERTEX_POINT ( 'NONE', #3361 ) ;
#7223 = ORIENTED_EDGE ( 'NONE', *, *, #2957, .T. ) ;
#7224 = EDGE_CURVE ( 'NONE', #12416, #6697, #928, .T. ) ;
#7225 = CIRCLE ( 'NONE', #5074, 6.500000000000005329 ) ;
#7226 = CARTESIAN_POINT ( 'NONE',  ( 229.9000000000000057, -4.577961614500551946, -3.910532886469501701 ) ) ;
#7227 = DIRECTION ( 'NONE',  ( 0.000000000000000000, 0.000000000000000000, 1.000000000000000000 ) ) ;
#7228 = CIRCLE ( 'NONE', #3808, 3.823498366181860231 ) ;
#7229 = CIRCLE ( 'NONE', #1695, 4.000000000000000000 ) ;
#7230 = CARTESIAN_POINT ( 'NONE',  ( 115.4648407705614090, 20.08915143315789109, 234.1947771724234713 ) ) ;
#7231 = DIRECTION ( 'NONE',  ( 0.6368676505102709440, 0.000000000000000000, 0.7709731485165532971 ) ) ;
#7232 = DIRECTION ( 'NONE',  ( 0.8660254037844380415, 0.000000000000000000, 0.5000000000000009992 ) ) ;
#7233 = CARTESIAN_POINT ( 'NONE',  ( -242.9798744223148788, 7.293926268967702242, 9.214525213515678104 ) ) ;
#7234 = PRODUCT_DEFINITION_SHAPE ( 'NONE', 'NONE',  #13089 ) ;
#7235 = AXIS2_PLACEMENT_3D ( 'NONE', #2495, #6572, #2368 ) ;
#7236 = ORIENTED_EDGE ( 'NONE', *, *, #12101, .F. ) ;
#7237 = DIRECTION ( 'NONE',  ( 0.000000000000000000, 0.000000000000000000, -1.000000000000000000 ) ) ;
#7238 = EDGE_LOOP ( 'NONE', ( #3617, #5904, #2017, #2771 ) ) ;
#7239 = CARTESIAN_POINT ( 'NONE',  ( 139.1326329530957082, -30.00000000000000000, -252.2620519511468729 ) ) ;
#7240 = ORIENTED_EDGE ( 'NONE', *, *, #4349, .F. ) ;
#7241 = ORIENTED_EDGE ( 'NONE', *, *, #12673, .F. ) ;
#7242 = DIRECTION ( 'NONE',  ( 0.000000000000000000, 1.000000000000000000, 0.000000000000000000 ) ) ;
#7243 =( NAMED_UNIT ( * ) PLANE_ANGLE_UNIT ( ) SI_UNIT ( $, .RADIAN. ) );
#7244 = DIRECTION ( 'NONE',  ( 0.6368676505102707219, 0.000000000000000000, 0.7709731485165536302 ) ) ;
#7245 = DIRECTION ( 'NONE',  ( -0.000000000000000000, -1.000000000000000000, 0.000000000000000000 ) ) ;
#7246 = LINE ( 'NONE', #9175, #6491 ) ;
#7247 = CARTESIAN_POINT ( 'NONE',  ( -290.6841825403030839, -19.00000000000000000, -27.68945685411394919 ) ) ;
#7248 = EDGE_LOOP ( 'NONE', ( #8551, #215, #11986, #7445 ) ) ;
#7249 = DIRECTION ( 'NONE',  ( 0.000000000000000000, 1.000000000000000000, 0.000000000000000000 ) ) ;
#7250 = EDGE_CURVE ( 'NONE', #2818, #12433, #8255, .T. ) ;
#7251 = ORIENTED_EDGE ( 'NONE', *, *, #7186, .F. ) ;
#7252 = CARTESIAN_POINT ( 'NONE',  ( 224.4939760857161843, 2.899436704890439476, -0.05715587751115609738 ) ) ;
#7253 = CARTESIAN_POINT ( 'NONE',  ( -243.4327047836247573, -7.689587473836074771, -9.212521827111036288 ) ) ;
#7254 = AXIS2_PLACEMENT_3D ( 'NONE', #7137, #8002, #12063 ) ;
#7255 = CARTESIAN_POINT ( 'NONE',  ( -249.7634162168646981, -11.48172779929090659, 2.515098141978860280 ) ) ;
#7256 = ORIENTED_EDGE ( 'NONE', *, *, #12017, .F. ) ;
#7257 = CARTESIAN_POINT ( 'NONE',  ( -67.61424743045878927, 20.79694577628127661, -252.4341100433800023 ) ) ;
#7258 = CARTESIAN_POINT ( 'NONE',  ( -242.3388033300362281, 6.664155345735165881, -9.979432606292707675 ) ) ;
#7259 = CARTESIAN_POINT ( 'NONE',  ( 122.2593324768334071, 18.00000000000000000, -168.2755348299895104 ) ) ;
#7260 = AXIS2_PLACEMENT_3D ( 'NONE', #5448, #5383, #324 ) ;
#7261 = CARTESIAN_POINT ( 'NONE',  ( -241.5784935629816914, -5.720435376789357207, -10.26436795190544515 ) ) ;
#7262 = ORIENTED_EDGE ( 'NONE', *, *, #519, .T. ) ;
#7263 = CARTESIAN_POINT ( 'NONE',  ( 239.2173603368114243, -1.070082897910355157, 3.332413334912896818 ) ) ;
#7264 = DIRECTION ( 'NONE',  ( 0.8042250444015808242, 0.5538822189107470706, -0.2154914511802788479 ) ) ;
#7265 = ADVANCED_FACE ( 'NONE', ( #10306 ), #11518, .T. ) ;
#7266 = CARTESIAN_POINT ( 'NONE',  ( -160.6180214586902650, 11.79660968244693997, -194.4394280558747710 ) ) ;
#7267 = ADVANCED_FACE ( 'NONE', ( #7317 ), #11384, .F. ) ;
#7268 = CARTESIAN_POINT ( 'NONE',  ( -197.8197553893909912, 30.00000000000000000, 64.27553482999130097 ) ) ;
#7269 = ORIENTED_EDGE ( 'NONE', *, *, #4487, .T. ) ;
#7270 = CIRCLE ( 'NONE', #458, 3.000000000000002665 ) ;
#7271 = CARTESIAN_POINT ( 'NONE',  ( -245.3956592407778601, 8.937419274608522812, -7.627912038536615924 ) ) ;
#7272 = CARTESIAN_POINT ( 'NONE',  ( 260.5542428351129729, 20.08915143297735284, 17.05314194231024771 ) ) ;
#7273 = LINE ( 'NONE', #11467, #6483 ) ;
#7274 = ADVANCED_FACE ( 'NONE', ( #7180 ), #12627, .T. ) ;
#7275 = CARTESIAN_POINT ( 'NONE',  ( 239.4141849552695192, -1.410389958860294168, -3.203344683049365926 ) ) ;
#7276 = CARTESIAN_POINT ( 'NONE',  ( 229.9000000000000057, 3.999223041228192610, -0.07883569311883599495 ) ) ;
#7277 = CARTESIAN_POINT ( 'NONE',  ( -250.0000000000000000, 0.000000000000000000, 0.000000000000000000 ) ) ;
#7278 = DIRECTION ( 'NONE',  ( 1.000000000000000000, 0.000000000000000000, 0.000000000000000000 ) ) ;
#7279 = DIRECTION ( 'NONE',  ( 0.9396926207859046531, 0.000000000000000000, 0.3420201433256790380 ) ) ;
#7280 = CARTESIAN_POINT ( 'NONE',  ( 290.6841825403032544, -19.00000000000000000, 27.68945685411186730 ) ) ;
#7281 =( REPRESENTATION_RELATIONSHIP ('NONE','NONE', #12019, #11596 ) REPRESENTATION_RELATIONSHIP_WITH_TRANSFORMATION ( #3576 )SHAPE_REPRESENTATION_RELATIONSHIP( ) );
#7282 = ORIENTED_EDGE ( 'NONE', *, *, #3957, .T. ) ;
#7283 = AXIS2_PLACEMENT_3D ( 'NONE', #2591, #1536, #6610 ) ;
#7284 = CARTESIAN_POINT ( 'NONE',  ( -122.2593324768359935, 19.00000000000000000, -162.7755348299880040 ) ) ;
#7285 = DIRECTION ( 'NONE',  ( 0.000000000000000000, 1.000000000000000000, 0.000000000000000000 ) ) ;
#7286 = ORIENTED_EDGE ( 'NONE', *, *, #7130, .F. ) ;
#7287 = ORIENTED_EDGE ( 'NONE', *, *, #2786, .T. ) ;
#7288 = DIRECTION ( 'NONE',  ( -0.000000000000000000, -1.000000000000000000, 0.000000000000000000 ) ) ;
#7289 = DIRECTION ( 'NONE',  ( 0.000000000000000000, 1.000000000000000000, 0.000000000000000000 ) ) ;
#7290 = ADVANCED_FACE ( 'NONE', ( #5243, #1313 ), #10370, .F. ) ;
#7291 = AXIS2_PLACEMENT_3D ( 'NONE', #1477, #4595, #1612 ) ;
#7292 = EDGE_CURVE ( 'NONE', #1505, #9162, #3252, .T. ) ;
#7293 = CARTESIAN_POINT ( 'NONE',  ( -226.7975291074607469, 20.55460285152577526, 130.9697226057901673 ) ) ;
#7294 = CARTESIAN_POINT ( 'NONE',  ( 0.000000000000000000, 0.000000000000000000, 0.000000000000000000 ) ) ;
#7295 = AXIS2_PLACEMENT_3D ( 'NONE', #1042, #980, #6052 ) ;
#7296 = CARTESIAN_POINT ( 'NONE',  ( -245.9694114402524576, 9.199502179615894448, 7.310239096702775718 ) ) ;
#7297 = EDGE_LOOP ( 'NONE', ( #7563, #2147, #7236, #3946 ) ) ;
#7298 = LINE ( 'NONE', #2285, #6265 ) ;
#7299 = EDGE_LOOP ( 'NONE', ( #5073, #10292, #3547, #7262 ) ) ;
#7300 = CARTESIAN_POINT ( 'NONE',  ( -289.8128292627096130, -18.00000000000000000, 10.41748504886635907 ) ) ;
#7301 = ORIENTED_EDGE ( 'NONE', *, *, #1156, .T. ) ;
#7302 = ORIENTED_EDGE ( 'NONE', *, *, #1227, .T. ) ;
#7303 = AXIS2_PLACEMENT_3D ( 'NONE', #11948, #8816, #6559 ) ;
#7304 = CIRCLE ( 'NONE', #1767, 196.0000000000000000 ) ;
#7305 = DIRECTION ( 'NONE',  ( 0.6368676505102689456, 0.000000000000000000, 0.7709731485165549625 ) ) ;
#7306 = EDGE_CURVE ( 'NONE', #11763, #12401, #9381, .T. ) ;
#7307 = DIRECTION ( 'NONE',  ( 0.000000000000000000, -1.000000000000000000, 0.000000000000000000 ) ) ;
#7308 = CARTESIAN_POINT ( 'NONE',  ( 0.000000000000000000, 1.848645179567965036, 0.000000000000000000 ) ) ;
#7309 = CARTESIAN_POINT ( 'NONE',  ( 227.3999999999999773, 0.000000000000000000, 0.000000000000000000 ) ) ;
#7310 = CARTESIAN_POINT ( 'NONE',  ( -239.2405828798147525, 1.531662351602087524, -11.64972450408488136 ) ) ;
#7311 = CARTESIAN_POINT ( 'NONE',  ( 3.039165139883816849E-14, 9.830508068699479907, -248.1666666666505137 ) ) ;
#7312 = AXIS2_PLACEMENT_3D ( 'NONE', #7889, #8691, #11705 ) ;
#7313 = CIRCLE ( 'NONE', #10282, 240.3921568627444856 ) ;
#7314 = CONTEXT_DEPENDENT_SHAPE_REPRESENTATION ( #9823, #2726 ) ;
#7315 = ORIENTED_EDGE ( 'NONE', *, *, #1735, .T. ) ;
#7316 = VECTOR ( 'NONE', #5427, 1000.000000000000000 ) ;
#7317 = FACE_OUTER_BOUND ( 'NONE', #663, .T. ) ;
#7318 = ORIENTED_EDGE ( 'NONE', *, *, #8372, .T. ) ;
#7319 = DIRECTION ( 'NONE',  ( 0.000000000000000000, 0.000000000000000000, 1.000000000000000000 ) ) ;
#7320 = CARTESIAN_POINT ( 'NONE',  ( -246.1949466613016284, -9.295128601147414571, -7.589564690491403809 ) ) ;
#7321 = CARTESIAN_POINT ( 'NONE',  ( 196.0019244007920918, 20.08915143297736350, 171.8850263962753218 ) ) ;
#7322 = ORIENTED_EDGE ( 'NONE', *, *, #683, .F. ) ;
#7323 = AXIS2_PLACEMENT_3D ( 'NONE', #5973, #901, #1903 ) ;
#7324 = CARTESIAN_POINT ( 'NONE',  ( -159.0697709846024850, 20.79694577629653551, -207.3438552932539949 ) ) ;
#7325 = CARTESIAN_POINT ( 'NONE',  ( -240.5462192425209764, 3.949737371798292873, -11.33143176614105307 ) ) ;
#7326 = CARTESIAN_POINT ( 'NONE',  ( -239.0198605536209868, 1.219845044661834521, 11.93783858050256796 ) ) ;
#7327 = CARTESIAN_POINT ( 'NONE',  ( -244.6792151818266916, -8.549823282788482359, -8.060814825372974113 ) ) ;
#7328 = LINE ( 'NONE', #4126, #3082 ) ;
#7329 = APPLICATION_PROTOCOL_DEFINITION ( 'draft international standard', 'automotive_design', 1998, #1834 ) ;
#7330 = CARTESIAN_POINT ( 'NONE',  ( -229.7138320264111258, 3.546086608952734753, -11.47018943898591559 ) ) ;
#7331 = AXIS2_PLACEMENT_3D ( 'NONE', #5033, #11109, #3099 ) ;
#7332 = CONTEXT_DEPENDENT_SHAPE_REPRESENTATION ( #5339, #7816 ) ;
#7333 = DIRECTION ( 'NONE',  ( 0.6368676505102709440, 0.000000000000000000, 0.7709731485165532971 ) ) ;
#7334 = EDGE_LOOP ( 'NONE', ( #9552, #2645, #9738, #8617 ) ) ;
#7335 = CARTESIAN_POINT ( 'NONE',  ( 158.9353507265259964, 20.08915143275230974, -207.1687172319319927 ) ) ;
#7336 = DIRECTION ( 'NONE',  ( 0.000000000000000000, 0.000000000000000000, 1.000000000000000000 ) ) ;
#7337 = ADVANCED_FACE ( 'NONE', ( #4112, #8192 ), #12251, .F. ) ;
#7338 = CARTESIAN_POINT ( 'NONE',  ( -249.3654635699440121, 10.61071050092431989, 5.052935794436599792 ) ) ;
#7339 = ADVANCED_FACE ( 'NONE', ( #10769 ), #2616, .F. ) ;
#7340 = PRODUCT_DEFINITION_SHAPE ( 'NONE', 'NONE',  #13093 ) ;
#7341 = LINE ( 'NONE', #8219, #2 ) ;
#7342 = CIRCLE ( 'NONE', #7135, 195.0000000000000000 ) ;
#7343 = FACE_OUTER_BOUND ( 'NONE', #5169, .T. ) ;
#7344 = FACE_OUTER_BOUND ( 'NONE', #9150, .T. ) ;
#7345 = CARTESIAN_POINT ( 'NONE',  ( 227.3999999999999773, 0.000000000000000000, 0.000000000000000000 ) ) ;
#7346 = CARTESIAN_POINT ( 'NONE',  ( 0.000000000000000000, 0.000000000000000000, 0.000000000000000000 ) ) ;
#7347 = CARTESIAN_POINT ( 'NONE',  ( -247.6398763846271436, -9.748465891248590864, 6.561428695831911462 ) ) ;
#7348 = CONTEXT_DEPENDENT_SHAPE_REPRESENTATION ( #1164, #5165 ) ;
#7349 = ORIENTED_EDGE ( 'NONE', *, *, #7529, .F. ) ;
#7350 = DIRECTION ( 'NONE',  ( 0.000000000000000000, 0.000000000000000000, 1.000000000000000000 ) ) ;
#7351 = PRODUCT_DEFINITION_SHAPE ( 'NONE', 'NONE',  #13050 ) ;
#7352 = CARTESIAN_POINT ( 'NONE',  ( 229.9983167069754018, -3.387876257721513351, 0.9084892790186469558 ) ) ;
#7353 = ORIENTED_EDGE ( 'NONE', *, *, #11124, .T. ) ;
#7354 = VERTEX_POINT ( 'NONE', #8769 ) ;
#7355 = CARTESIAN_POINT ( 'NONE',  ( 159.6627199829248411, -25.00000000000000000, 193.2829683331000012 ) ) ;
#7356 = CARTESIAN_POINT ( 'NONE',  ( 11.00000000000000000, 0.000000000000000000, 250.0000000000000000 ) ) ;
#7357 = UNCERTAINTY_MEASURE_WITH_UNIT (LENGTH_MEASURE( 1.000000000000000082E-05 ), #9033, 'distance_accuracy_value', 'NONE');
#7358 = CARTESIAN_POINT ( 'NONE',  ( 259.4723857435290597, 19.96883745944077404, 34.18476129351889625 ) ) ;
#7359 = AXIS2_PLACEMENT_3D ( 'NONE', #5455, #4573, #653 ) ;
#7360 = DIRECTION ( 'NONE',  ( 0.000000000000000000, 0.000000000000000000, 1.000000000000000000 ) ) ;
#7361 = CARTESIAN_POINT ( 'NONE',  ( 0.000000000000000000, 0.000000000000000000, 0.000000000000000000 ) ) ;
#7362 = AXIS2_PLACEMENT_3D ( 'NONE', #233, #4292, #8374 ) ;
#7363 = CARTESIAN_POINT ( 'NONE',  ( 0.000000000000000000, 21.99999999999995381, -246.0000000000000000 ) ) ;
#7364 = ORIENTED_EDGE ( 'NONE', *, *, #3681, .F. ) ;
#7365 = CARTESIAN_POINT ( 'NONE',  ( -122.2593324768359935, 19.00000000000000000, -168.2755348299880040 ) ) ;
#7366 = EDGE_CURVE ( 'NONE', #6584, #10501, #3465, .T. ) ;
#7367 = ORIENTED_EDGE ( 'NONE', *, *, #11245, .T. ) ;
#7368 = ADVANCED_FACE ( 'NONE', ( #5701 ), #4622, .F. ) ;
#7369 = DIRECTION ( 'NONE',  ( 0.000000000000000000, 0.000000000000000000, -1.000000000000000000 ) ) ;
#7370 = ORIENTED_EDGE ( 'NONE', *, *, #59, .T. ) ;
#7371 = ORIENTED_EDGE ( 'NONE', *, *, #2724, .T. ) ;
#7372 = CARTESIAN_POINT ( 'NONE',  ( -5.000000000000000000, 0.000000000000000000, 258.0000000000000000 ) ) ;
#7373 = FACE_BOUND ( 'NONE', #10035, .T. ) ;
#7374 = DIRECTION ( 'NONE',  ( -0.000000000000000000, -1.000000000000000000, 0.000000000000000000 ) ) ;
#7375 = CARTESIAN_POINT ( 'NONE',  ( 239.0693672987491425, 0.6815372134079659139, -3.433431997376373168 ) ) ;
#7376 = DIRECTION ( 'NONE',  ( -0.000000000000000000, 0.01970892327970912364, 0.9998057603070482635 ) ) ;
#7377 = CARTESIAN_POINT ( 'NONE',  ( -247.0556047488532840, 9.588534006617832617, 7.215007616888431841 ) ) ;
#7378 = ORIENTED_EDGE ( 'NONE', *, *, #9789, .F. ) ;
#7379 = CARTESIAN_POINT ( 'NONE',  ( -197.8197553893924976, 30.00000000000000000, -64.27553482998719403 ) ) ;
#7380 = EDGE_LOOP ( 'NONE', ( #7802, #7589 ) ) ;
#7381 = EDGE_CURVE ( 'NONE', #1937, #2804, #10830, .T. ) ;
#7382 = DIRECTION ( 'NONE',  ( 0.000000000000000000, 1.000000000000000000, 0.000000000000000000 ) ) ;
#7383 = DIRECTION ( 'NONE',  ( -0.6368676505102707219, 0.000000000000000000, -0.7709731485165535192 ) ) ;
#7384 = CARTESIAN_POINT ( 'NONE',  ( 107.5873595010541948, 20.08915143297735995, 237.4577367525702982 ) ) ;
#7385 = EDGE_LOOP ( 'NONE', ( #27, #8837 ) ) ;
#7386 = EDGE_CURVE ( 'NONE', #10752, #2886, #2565, .T. ) ;
#7387 = PLANE ( 'NONE',  #10850 ) ;
#7388 = CARTESIAN_POINT ( 'NONE',  ( -242.5248711414777461, 6.860954770765020250, -9.845341009612386785 ) ) ;
#7389 = CARTESIAN_POINT ( 'NONE',  ( -239.8750565987691061, 2.115697798598445978, 11.81209311377322813 ) ) ;
#7390 = CARTESIAN_POINT ( 'NONE',  ( -241.2214908400834474, -5.194817168110312799, -10.54181336083197884 ) ) ;
#7391 = CARTESIAN_POINT ( 'NONE',  ( 239.0883580246742781, -0.7438334348235525750, 3.420275401449059505 ) ) ;
#7392 = DIRECTION ( 'NONE',  ( 0.07256543843574699004, 0.5538822189107472926, 0.8294267566935222824 ) ) ;
#7393 = CARTESIAN_POINT ( 'NONE',  ( -229.8079896091062153, 7.470059805363084671, -9.398818199247862992 ) ) ;
#7394 = DIRECTION ( 'NONE',  ( -0.6368676505102700558, 0.000000000000000000, -0.7709731485165541853 ) ) ;
#7395 = ORIENTED_EDGE ( 'NONE', *, *, #5705, .F. ) ;
#7396 = CONICAL_SURFACE ( 'NONE', #1645, 5.500000000000005329, 0.7853981633974461696 ) ;
#7397 = CARTESIAN_POINT ( 'NONE',  ( 226.1171533156415023, 20.08915143315739726, 130.5770120865019805 ) ) ;
#7398 = FACE_BOUND ( 'NONE', #37, .T. ) ;
#7399 = DIRECTION ( 'NONE',  ( 0.5469441386039890496, 0.000000000000000000, -0.8371691043312220470 ) ) ;
#7400 = CARTESIAN_POINT ( 'NONE',  ( 235.0999999999999943, 0.000000000000000000, 0.000000000000000000 ) ) ;
#7401 = DIRECTION ( 'NONE',  ( 0.000000000000000000, -1.000000000000000000, 0.000000000000000000 ) ) ;
#7402 = DIRECTION ( 'NONE',  ( 0.000000000000000000, 0.000000000000000000, -1.000000000000000000 ) ) ;
#7403 = DIRECTION ( 'NONE',  ( -0.8199460427888404235, 0.5538822189107471816, 0.1445786100688074838 ) ) ;
#7404 = DIRECTION ( 'NONE',  ( -0.000000000000000000, -1.000000000000000000, 0.000000000000000000 ) ) ;
#7405 = CONTEXT_DEPENDENT_SHAPE_REPRESENTATION ( #2855, #6767 ) ;
#7406 = VERTEX_POINT ( 'NONE', #9507 ) ;
#7407 =( REPRESENTATION_RELATIONSHIP ('NONE','NONE', #12019, #5191 ) REPRESENTATION_RELATIONSHIP_WITH_TRANSFORMATION ( #6532 )SHAPE_REPRESENTATION_RELATIONSHIP( ) );
#7408 = LINE ( 'NONE', #11416, #11516 ) ;
#7409 = EDGE_CURVE ( 'NONE', #5526, #3236, #294, .T. ) ;
#7410 = DIRECTION ( 'NONE',  ( 0.6368676505102737195, 0.000000000000000000, 0.7709731485165509657 ) ) ;
#7411 = ORIENTED_EDGE ( 'NONE', *, *, #428, .T. ) ;
#7412 = ORIENTED_EDGE ( 'NONE', *, *, #8940, .F. ) ;
#7413 = CYLINDRICAL_SURFACE ( 'NONE', #2300, 5.500000000000005329 ) ;
#7414 = SPHERICAL_SURFACE ( 'NONE', #3116, 9.900000000000000355 ) ;
#7415 = TOROIDAL_SURFACE ( 'NONE', #7836, 241.5000000000000000, 2.500000000000000000 ) ;
#7416 = AXIS2_PLACEMENT_3D ( 'NONE', #5135, #2140, #11344 ) ;
#7417 = CARTESIAN_POINT ( 'NONE',  ( 207.6469600138280498, 19.96883746145561389, 159.3024069661363740 ) ) ;
#7418 = DIRECTION ( 'NONE',  ( 0.000000000000000000, 0.000000000000000000, 1.000000000000000000 ) ) ;
#7419 = DIRECTION ( 'NONE',  ( -0.4999999999999949485, 0.000000000000000000, -0.8660254037844415942 ) ) ;
#7420 = CARTESIAN_POINT ( 'NONE',  ( 0.000000000000000000, 24.99999999999995737, 0.000000000000000000 ) ) ;
#7421 = CARTESIAN_POINT ( 'NONE',  ( -8.533827019710209072, 20.79694577634647601, 260.7745447061713548 ) ) ;
#7422 = ORIENTED_EDGE ( 'NONE', *, *, #12346, .T. ) ;
#7423 = TOROIDAL_SURFACE ( 'NONE', #1676, 250.0000000000000000, 10.00000000000000000 ) ;
#7424 = DIRECTION ( 'NONE',  ( 0.000000000000000000, 1.000000000000000000, 0.000000000000000000 ) ) ;
#7425 = EDGE_CURVE ( 'NONE', #4744, #1370, #3563, .T. ) ;
#7427 = ORIENTED_EDGE ( 'NONE', *, *, #4918, .F. ) ;
#7426 = CIRCLE ( 'NONE', #1679, 5.500000000000015099 ) ;
#7428 = VECTOR ( 'NONE', #3882, 1000.000000000000000 ) ;
#7429 = CARTESIAN_POINT ( 'NONE',  ( -122.2593324768321992, 19.00000000000000000, 162.7755348299905052 ) ) ;
#7430 = ORIENTED_EDGE ( 'NONE', *, *, #2712, .T. ) ;
#7431 = ORIENTED_EDGE ( 'NONE', *, *, #11711, .F. ) ;
#7432 = AXIS2_PLACEMENT_3D ( 'NONE', #6325, #5316, #254 ) ;
#7433 = AXIS2_PLACEMENT_3D ( 'NONE', #9652, #8404, #5460 ) ;
#7434 = FACE_OUTER_BOUND ( 'NONE', #10725, .T. ) ;
#7435 = PLANE ( 'NONE',  #7235 ) ;
#7436 = EDGE_CURVE ( 'NONE', #3272, #11832, #7104, .T. ) ;
#7437 = CARTESIAN_POINT ( 'NONE',  ( 238.9743710159888224, -9.335707311080796797E-14, -3.499999942258349428 ) ) ;
#7438 = VECTOR ( 'NONE', #1713, 1000.000000000000000 ) ;
#7439 = CARTESIAN_POINT ( 'NONE',  ( -238.7322507464853629, 0.3342974598293207422, -11.74538363270618468 ) ) ;
#7440 = CARTESIAN_POINT ( 'NONE',  ( -244.7822625628474213, 8.616351828725139939, 8.352152985389436068 ) ) ;
#7441 = DIRECTION ( 'NONE',  ( 0.000000000000000000, 0.000000000000000000, -1.000000000000000000 ) ) ;
#7442 = VECTOR ( 'NONE', #5299, 1000.000000000000227 ) ;
#7443 = EDGE_LOOP ( 'NONE', ( #9694, #12100, #7572, #6094 ) ) ;
#7444 = DIRECTION ( 'NONE',  ( 0.6368676505102707219, 0.000000000000000000, 0.7709731485165535192 ) ) ;
#7445 = ORIENTED_EDGE ( 'NONE', *, *, #1492, .F. ) ;
#7446 = DIRECTION ( 'NONE',  ( 0.000000000000000000, 1.000000000000000000, 0.000000000000000000 ) ) ;
#7447 = DIRECTION ( 'NONE',  ( 0.000000000000000000, 0.9998057603070480415, -0.01970892327970899874 ) ) ;
#7448 = CIRCLE ( 'NONE', #9148, 1.949999999999999734 ) ;
#7449 = CARTESIAN_POINT ( 'NONE',  ( 130.3442252640566039, 20.08915143297736705, -225.7689075324036025 ) ) ;
#7450 = ORIENTED_EDGE ( 'NONE', *, *, #11353, .F. ) ;
#7451 = CIRCLE ( 'NONE', #1064, 254.0000000000000000 ) ;
#7452 = CARTESIAN_POINT ( 'NONE',  ( -240.1208361041844910, -2.772967769359084844, -11.41810622433049893 ) ) ;
#7453 = CARTESIAN_POINT ( 'NONE',  ( -242.4607547118677076, 6.794574172261055089, -9.891349720023484338 ) ) ;
#7454 = CARTESIAN_POINT ( 'NONE',  ( -239.0779495979048477, 1.320275893629169639, 11.92738862982784021 ) ) ;
#7455 = ADVANCED_FACE ( 'NONE', ( #11840 ), #12576, .F. ) ;
#7456 = CARTESIAN_POINT ( 'NONE',  ( -240.2602214610158455, -3.236828995517413876, -11.30545424822241252 ) ) ;
#7457 = ADVANCED_FACE ( 'NONE', ( #2628 ), #12215, .T. ) ;
#7458 = CONICAL_SURFACE ( 'NONE', #6398, 196.0000000000000000, 0.7853981633974758125 ) ;
#7459 = CARTESIAN_POINT ( 'NONE',  ( 239.4793126110744197, -1.500292815854004980, 3.162144597934753332 ) ) ;
#7460 = PRODUCT_DEFINITION_SHAPE ( 'NONE', 'NONE',  #13054 ) ;
#7461 = PRODUCT_CONTEXT ( 'NONE', #7982, 'mechanical' ) ;
#7462 = CARTESIAN_POINT ( 'NONE',  ( 235.0999999999999943, 2.749465840844381948, -0.05419953901919974393 ) ) ;
#7463 = ADVANCED_FACE ( 'NONE', ( #6518 ), #4747, .F. ) ;
#7464 = AXIS2_PLACEMENT_3D ( 'NONE', #2469, #8544, #9411 ) ;
#7465 = DIRECTION ( 'NONE',  ( 0.000000000000000000, -0.3950277506594045973, -0.9186691875800402363 ) ) ;
#7466 = VERTEX_POINT ( 'NONE', #6715 ) ;
#7467 = CARTESIAN_POINT ( 'NONE',  ( 84.14846197943569450, 19.96883746176665397, 247.8175805191055190 ) ) ;
#7468 = CARTESIAN_POINT ( 'NONE',  ( 122.2593324768346008, 30.00000000000000000, 174.7755348299889988 ) ) ;
#7469 = DIRECTION ( 'NONE',  ( 0.000000000000000000, 1.000000000000000000, 0.000000000000000000 ) ) ;
#7470 = DIRECTION ( 'NONE',  ( 1.000000000000000000, 0.000000000000000000, 0.000000000000000000 ) ) ;
#7471 = EDGE_LOOP ( 'NONE', ( #12950, #1079, #7785, #1795 ) ) ;
#7472 = ADVANCED_FACE ( 'NONE', ( #1634 ), #9564, .F. ) ;
#7473 = CARTESIAN_POINT ( 'NONE',  ( 0.000000000000000000, -11.79660968244690089, 247.7999999999999829 ) ) ;
#7474 = DIRECTION ( 'NONE',  ( 0.000000000000000000, -1.000000000000000000, 0.000000000000000000 ) ) ;
#7475 = DIRECTION ( 'NONE',  ( -0.4775568914688836375, 0.5538822189107472926, 0.6820219226572444837 ) ) ;
#7476 = DIRECTION ( 'NONE',  ( -0.000000000000000000, -1.000000000000000000, 0.000000000000000000 ) ) ;
#7477 = CONTEXT_DEPENDENT_SHAPE_REPRESENTATION ( #11731, #8165 ) ;
#7478 = LINE ( 'NONE', #3134, #1077 ) ;
#7479 = AXIS2_PLACEMENT_3D ( 'NONE', #976, #8976, #3904 ) ;
#7480 = CARTESIAN_POINT ( 'NONE',  ( -239.1867390642027544, -1.460152697550930689, 11.65892209769657661 ) ) ;
#7481 = CIRCLE ( 'NONE', #7025, 5.500000000000007994 ) ;
#7482 = CARTESIAN_POINT ( 'NONE',  ( -229.8469569043687670, -8.584093440156065569, 8.393536236380878535 ) ) ;
#7483 = ORIENTED_EDGE ( 'NONE', *, *, #12569, .T. ) ;
#7484 = EDGE_LOOP ( 'NONE', ( #12168, #1556 ) ) ;
#7485 = CYLINDRICAL_SURFACE ( 'NONE', #604, 5.500000000000015099 ) ;
#7486 = FACE_BOUND ( 'NONE', #5104, .T. ) ;
#7487 = TOROIDAL_SURFACE ( 'NONE', #11958, 250.0000000000000000, 10.00000000000000000 ) ;
#7488 = CARTESIAN_POINT ( 'NONE',  ( -130.9697226053157237, 20.55460285097016282, -226.7975291069864738 ) ) ;
#7489 = ORIENTED_EDGE ( 'NONE', *, *, #12302, .F. ) ;
#7490 = CARTESIAN_POINT ( 'NONE',  ( 0.000000000000000000, 0.000000000000000000, 0.000000000000000000 ) ) ;
#7491 = CARTESIAN_POINT ( 'NONE',  ( 0.000000000000000000, 0.000000000000000000, 0.000000000000000000 ) ) ;
#7492 =( REPRESENTATION_RELATIONSHIP ('NONE','NONE', #12019, #5191 ) REPRESENTATION_RELATIONSHIP_WITH_TRANSFORMATION ( #8211 )SHAPE_REPRESENTATION_RELATIONSHIP( ) );
#7493 = CARTESIAN_POINT ( 'NONE',  ( 222.0845275804282153, 0.000000000000000000, 0.000000000000000000 ) ) ;
#7494 = CARTESIAN_POINT ( 'NONE',  ( -234.0054343868620208, 20.79694577634646535, 115.4021059068214896 ) ) ;
#7495 = EDGE_LOOP ( 'NONE', ( #10828, #5541, #2959, #10129 ) ) ;
#7496 = CARTESIAN_POINT ( 'NONE',  ( 67.53249125288877508, 20.79694577634646180, -252.0229195836992062 ) ) ;
#7497 = ORIENTED_EDGE ( 'NONE', *, *, #5468, .F. ) ;
#7498 = CYLINDRICAL_SURFACE ( 'NONE', #7635, 5.100000000000000533 ) ;
#7499 = ORIENTED_EDGE ( 'NONE', *, *, #3915, .F. ) ;
#7500 = EDGE_LOOP ( 'NONE', ( #8616, #12609, #1193, #7489 ) ) ;
#7501 = VECTOR ( 'NONE', #1736, 1000.000000000000000 ) ;
#7502 = LINE ( 'NONE', #9440, #4526 ) ;
#7503 = CARTESIAN_POINT ( 'NONE',  ( 290.6841825403032544, -18.00000000000000000, 27.68945685411186730 ) ) ;
#7504 = CIRCLE ( 'NONE', #1972, 8.000000000000007105 ) ;
#7505 = EDGE_CURVE ( 'NONE', #6601, #10050, #8989, .T. ) ;
#7506 = EDGE_CURVE ( 'NONE', #8008, #4210, #8175, .T. ) ;
#7507 = DIRECTION ( 'NONE',  ( 0.6368676505102716101, 0.000000000000000000, 0.7709731485165527420 ) ) ;
#7508 = CARTESIAN_POINT ( 'NONE',  ( -239.1986688623609325, 1.476435535276028110, -11.65686989423240938 ) ) ;
#7509 = ITEM_DEFINED_TRANSFORMATION ( 'NONE', 'NONE', #5711,  #805 ) ;
#7510 = ORIENTED_EDGE ( 'NONE', *, *, #790, .T. ) ;
#7511 = CARTESIAN_POINT ( 'NONE',  ( 235.4000000000000057, 0.000000000000000000, 0.000000000000000000 ) ) ;
#7512 = AXIS2_PLACEMENT_3D ( 'NONE', #5425, #6428, #3339 ) ;
#7513 = ORIENTED_EDGE ( 'NONE', *, *, #1270, .T. ) ;
#7514 = CIRCLE ( 'NONE', #11562, 5.499999999999986677 ) ;
#7515 = CARTESIAN_POINT ( 'NONE',  ( -243.9217790931375305, 8.053804838624140316, -8.555499775521546724 ) ) ;
#7516 = DIRECTION ( 'NONE',  ( 0.000000000000000000, 0.000000000000000000, 1.000000000000000000 ) ) ;
#7517 = CARTESIAN_POINT ( 'NONE',  ( 237.4577367525703835, 20.08915143297736350, 107.5873595010540669 ) ) ;
#7518 = DIRECTION ( 'NONE',  ( -0.4503334343941627904, -0.7071067811865381358, -0.5451603414288054283 ) ) ;
#7519 = CARTESIAN_POINT ( 'NONE',  ( -242.6565958084028125, 6.994822115566234899, -9.751204002521671299 ) ) ;
#7520 = CARTESIAN_POINT ( 'NONE',  ( -238.7769902278642462, 0.6179568203354762757, 11.98408500534410948 ) ) ;
#7521 = CONICAL_SURFACE ( 'NONE', #11132, 261.0000000000000000, 1.373400766945014784 ) ;
#7522 = FACE_OUTER_BOUND ( 'NONE', #11151, .T. ) ;
#7523 = CONICAL_SURFACE ( 'NONE', #12000, 6.500000000000005329, 0.7853981633974476129 ) ;
#7524 = CLOSED_SHELL ( 'NONE', ( #346, #12600 ) ) ;
#7525 = FACE_OUTER_BOUND ( 'NONE', #105, .T. ) ;
#7526 =( LENGTH_UNIT ( ) NAMED_UNIT ( * ) SI_UNIT ( .MILLI., .METRE. ) );
#7527 = CARTESIAN_POINT ( 'NONE',  ( -229.8466722354996534, 8.576484730279149815, 8.401311290977700352 ) ) ;
#7528 = ADVANCED_FACE ( 'NONE', ( #4761 ), #5830, .F. ) ;
#7529 = EDGE_CURVE ( 'NONE', #9614, #5812, #2196, .T. ) ;
#7530 = CARTESIAN_POINT ( 'NONE',  ( 197.8197553893920144, 29.00000000000000000, 64.27553482998850143 ) ) ;
#7531 = ORIENTED_EDGE ( 'NONE', *, *, #2315, .T. ) ;
#7532 = CARTESIAN_POINT ( 'NONE',  ( -67.71318189764485851, 19.96883746024804651, -252.8031682270704437 ) ) ;
#7533 = DIRECTION ( 'NONE',  ( -0.000000000000000000, -1.000000000000000000, 0.000000000000000000 ) ) ;
#7534 = CARTESIAN_POINT ( 'NONE',  ( 221.6213872890270977, -29.00000000000000000, -190.2057062658400923 ) ) ;
#7535 =( REPRESENTATION_RELATIONSHIP ('NONE','NONE', #12019, #182 ) REPRESENTATION_RELATIONSHIP_WITH_TRANSFORMATION ( #4776 )SHAPE_REPRESENTATION_RELATIONSHIP( ) );
#7536 = DIRECTION ( 'NONE',  ( 0.000000000000000000, 0.000000000000000000, 1.000000000000000000 ) ) ;
#7537 = CARTESIAN_POINT ( 'NONE',  ( -253.8843055347118707, 20.08915143297737060, -59.19439222780466991 ) ) ;
#7538 = CONICAL_SURFACE ( 'NONE', #3485, 6.500000000000005329, 0.7853981633974518317 ) ;
#7539 = DIRECTION ( 'NONE',  ( -0.000000000000000000, -1.000000000000000000, 0.000000000000000000 ) ) ;
#7540 = DIRECTION ( 'NONE',  ( 0.7660444431189770143, 0.000000000000000000, 0.6427876096865404731 ) ) ;
#7541 = CARTESIAN_POINT ( 'NONE',  ( 0.000000000000000000, 24.99999999999995737, 0.000000000000000000 ) ) ;
#7542 = B_SPLINE_CURVE_WITH_KNOTS ( 'NONE', 3,
 ( #5520, #7984, #12373, #5785, #12979, #4975, #5986, #5035, #12048, #8851, #5918, #3972, #885, #6054, #9845, #12178, #4041, #8049, #1980, #11043, #7050, #2833, #918, #3842, #5855, #6852, #10108, #7842, #4838, #8117, #9914, #4775, #9982, #981, #9047, #851, #10845, #9110, #7911, #10912, #2898, #6788, #1717, #11111 ),
 .UNSPECIFIED., .F., .F.,
 ( 4, 2, 2, 2, 2, 2, 2, 1, 1, 1, 2, 2, 2, 2, 1, 1, 2, 2, 2, 2, 1, 2, 2, 2, 4 ),
 ( 0.000000000000000000, 0.06252861007222769441, 0.07034468633125084969, 0.07425272446076752741, 0.07816076259028420514, 0.09379291510834281143, 0.1094250676264014316, 0.1172411438854389504, 0.1211491820149575849, 0.1231032010797020321, 0.1240802106120912213, 0.1250572201444804243, 0.1875858302175758274, 0.2188501352541234735, 0.2344822877723924670, 0.2422983640315269638, 0.2462064021610991527, 0.2501144402906713138, 0.3126430503639207048, 0.3439073554005454558, 0.3595395079188577481, 0.3673555841780140052, 0.3751716604371702068, 0.4377002705104277580, 0.5002288805836853092 ),
 .UNSPECIFIED. ) ;
#7543 = AXIS2_PLACEMENT_3D ( 'NONE', #7833, #8651, #2634 ) ;
#7544 = CARTESIAN_POINT ( 'NONE',  ( -241.9271341488148153, -6.190796897788312769, -10.28045873088825957 ) ) ;
#7545 = EDGE_CURVE ( 'NONE', #1703, #90, #7114, .T. ) ;
#7546 = CARTESIAN_POINT ( 'NONE',  ( -229.7189907529219681, -3.915537799265266017, 11.36770974954495195 ) ) ;
#7547 = ORIENTED_EDGE ( 'NONE', *, *, #8205, .F. ) ;
#7548 = EDGE_LOOP ( 'NONE', ( #8199, #2179, #4534, #10020 ) ) ;
#7549 = CONICAL_SURFACE ( 'NONE', #8403, 6.500000000000005329, 0.7853981633974476129 ) ;
#7550 = DIRECTION ( 'NONE',  ( -0.000000000000000000, 1.000000000000000000, 0.000000000000000000 ) ) ;
#7551 = DIRECTION ( 'NONE',  ( -0.000000000000000000, 1.000000000000000000, 0.000000000000000000 ) ) ;
#7552 = EDGE_CURVE ( 'NONE', #10483, #9653, #9964, .T. ) ;
#7553 = CARTESIAN_POINT ( 'NONE',  ( -247.9906035374705766, 20.55460285117394648, 84.20717312385856701 ) ) ;
#7554 = DIRECTION ( 'NONE',  ( 8.659560562354926695E-17, 0.7071067811865480168, -0.7071067811865470176 ) ) ;
#7555 = DIRECTION ( 'NONE',  ( -0.8191520442889893561, 0.000000000000000000, -0.5735764363510499342 ) ) ;
#7556 = DIRECTION ( 'NONE',  ( 0.000000000000000000, 1.000000000000000000, 0.000000000000000000 ) ) ;
#7557 = CARTESIAN_POINT ( 'NONE',  ( -4.572608844893758122E-13, 20.79694577634647601, 260.7745447061711275 ) ) ;
#7558 = TOROIDAL_SURFACE ( 'NONE', #8619, 252.1999999999999886, 2.000000000000000000 ) ;
#7559 = EDGE_LOOP ( 'NONE', ( #10326, #9799, #9740, #11434 ) ) ;
#7560 = CARTESIAN_POINT ( 'NONE',  ( -233.0000000000000000, 1.000000000000000000, -11.95826074310140008 ) ) ;
#7561 = ORIENTED_EDGE ( 'NONE', *, *, #1227, .F. ) ;
#7562 = LINE ( 'NONE', #3487, #12110 ) ;
#7563 = ORIENTED_EDGE ( 'NONE', *, *, #9863, .T. ) ;
#7564 = ORIENTED_EDGE ( 'NONE', *, *, #3117, .T. ) ;
#7565 = CARTESIAN_POINT ( 'NONE',  ( 0.000000000000000000, 19.00000000000000000, 0.000000000000000000 ) ) ;
#7566 = FACE_OUTER_BOUND ( 'NONE', #9135, .T. ) ;
#7567 = VECTOR ( 'NONE', #5227, 1000.000000000000000 ) ;
#7568 = CARTESIAN_POINT ( 'NONE',  ( 239.4068548684666951, 1.402387639960759103, -3.207804078284339777 ) ) ;
#7569 = CYLINDRICAL_SURFACE ( 'NONE', #6061, 305.0000000000000000 ) ;
#7570 = CARTESIAN_POINT ( 'NONE',  ( 0.000000000000000000, 0.000000000000000000, -250.0000000000000000 ) ) ;
#7571 = FACE_OUTER_BOUND ( 'NONE', #2538, .T. ) ;
#7572 = ORIENTED_EDGE ( 'NONE', *, *, #2530, .T. ) ;
#7573 = CARTESIAN_POINT ( 'NONE',  ( 130.7196491263533744, -23.50000000000000000, -200.0834159351620656 ) ) ;
#7574 = AXIS2_PLACEMENT_3D ( 'NONE', #12778, #9578, #3714 ) ;
#7575 = ORIENTED_EDGE ( 'NONE', *, *, #107, .F. ) ;
#7576 = CARTESIAN_POINT ( 'NONE',  ( -240.2520669369037023, 3.209691513938345064, -11.31204477735925451 ) ) ;
#7577 = CARTESIAN_POINT ( 'NONE',  ( 224.4939760857161843, 0.000000000000000000, 0.000000000000000000 ) ) ;
#7578 = EDGE_CURVE ( 'NONE', #5226, #3634, #11367, .T. ) ;
#7579 = VECTOR ( 'NONE', #1876, 1000.000000000000227 ) ;
#7580 = CARTESIAN_POINT ( 'NONE',  ( 0.000000000000000000, 21.99999999999995381, 0.000000000000000000 ) ) ;
#7581 = LINE ( 'NONE', #8776, #9250 ) ;
#7582 = CARTESIAN_POINT ( 'NONE',  ( -238.7702306800076428, 0.5911393334065133676, 11.98543574551528401 ) ) ;
#7583 = CARTESIAN_POINT ( 'NONE',  ( -229.8106098029694522, 7.168838942085261401, 9.341759543542826449 ) ) ;
#7584 = CARTESIAN_POINT ( 'NONE',  ( -246.0505219340116980, -9.238338704761243747, 7.658960895840565719 ) ) ;
#7585 = DIRECTION ( 'NONE',  ( 0.6368676505102707219, 0.000000000000000000, 0.7709731485165535192 ) ) ;
#7586 = APPLICATION_PROTOCOL_DEFINITION ( 'draft international standard', 'automotive_design', 1998, #12301 ) ;
#7587 = CARTESIAN_POINT ( 'NONE',  ( -229.9997784648330708, 11.99578910728947712, -0.3697823523935888090 ) ) ;
#7588 = ADVANCED_FACE ( 'NONE', ( #8103 ), #6910, .F. ) ;
#7589 = ORIENTED_EDGE ( 'NONE', *, *, #2456, .F. ) ;
#7590 = CARTESIAN_POINT ( 'NONE',  ( 0.000000000000000000, 0.000000000000000000, -249.7999999999999829 ) ) ;
#7591 = EDGE_LOOP ( 'NONE', ( #7883, #9271 ) ) ;
#7592 = CARTESIAN_POINT ( 'NONE',  ( -172.5787240293117293, 19.96883745935916821, -196.7513681803530403 ) ) ;
#7593 = DIRECTION ( 'NONE',  ( 0.000000000000000000, 1.000000000000000000, 0.000000000000000000 ) ) ;
#7594 = CARTESIAN_POINT ( 'NONE',  ( 185.9653539490014111, -19.00000000000000000, 225.1241593668316625 ) ) ;
#7595 = DIRECTION ( 'NONE',  ( 1.000000000000000000, 0.000000000000000000, 0.000000000000000000 ) ) ;
#7596 = CARTESIAN_POINT ( 'NONE',  ( -251.8100110699625418, 20.08915143297736705, 67.47543992451960548 ) ) ;
#7597 = EDGE_CURVE ( 'NONE', #2539, #11365, #9036, .T. ) ;
#7598 = EDGE_CURVE ( 'NONE', #1614, #3781, #3017, .T. ) ;
#7599 = DIRECTION ( 'NONE',  ( 0.000000000000000000, -1.000000000000000000, 0.000000000000000000 ) ) ;
#7600 = AXIS2_PLACEMENT_3D ( 'NONE', #10607, #11423, #9602 ) ;
#7601 = DIRECTION ( 'NONE',  ( -0.6378047977532539381, 0.5538822189107472926, 0.5351817705578529871 ) ) ;
#7602 = CARTESIAN_POINT ( 'NONE',  ( -229.8401422497489932, -8.039079579276160459, -8.578028158269177084 ) ) ;
#7603 = CONTEXT_DEPENDENT_SHAPE_REPRESENTATION ( #11126, #1643 ) ;
#7604 = DIRECTION ( 'NONE',  ( 8.659560562354926695E-17, -0.7071067811865480168, 0.7071067811865470176 ) ) ;
#7605 = VECTOR ( 'NONE', #1661, 999.9999999999998863 ) ;
#7606 = CARTESIAN_POINT ( 'NONE',  ( -229.8371538172024771, -8.318415249073295215, 8.657075633561293060 ) ) ;
#7607 = ORIENTED_EDGE ( 'NONE', *, *, #10355, .F. ) ;
#7608 = ORIENTED_EDGE ( 'NONE', *, *, #11421, .T. ) ;
#7609 = CARTESIAN_POINT ( 'NONE',  ( 227.3999999999999773, -4.550331206106116078, -2.508881407069070590 ) ) ;
#7610 = CARTESIAN_POINT ( 'NONE',  ( 190.1049936773181628, -30.00000000000000000, 230.1354848321892632 ) ) ;
#7611 = EDGE_CURVE ( 'NONE', #1691, #12854, #4972, .T. ) ;
#7612 = CARTESIAN_POINT ( 'NONE',  ( 172.6991790965608971, 20.55460285089974093, 196.8887528236631965 ) ) ;
#7613 =( GEOMETRIC_REPRESENTATION_CONTEXT ( 3 ) GLOBAL_UNCERTAINTY_ASSIGNED_CONTEXT ( ( #2899 ) ) GLOBAL_UNIT_ASSIGNED_CONTEXT ( ( #10895, #3893, #1771 ) ) REPRESENTATION_CONTEXT ( 'NONE', 'WORKASPACE' ) );
#7614 = EDGE_CURVE ( 'NONE', #10097, #2361, #12901, .T. ) ;
#7615 = DIRECTION ( 'NONE',  ( 0.000000000000000000, 0.9998057603070481525, -0.01970892327970900221 ) ) ;
#7616 = DIRECTION ( 'NONE',  ( 0.2588190451025179639, 0.000000000000000000, 0.9659258262890690894 ) ) ;
#7617 = CARTESIAN_POINT ( 'NONE',  ( 5.000000000000000000, 0.000000000000000000, 258.0000000000000000 ) ) ;
#7618 = DIRECTION ( 'NONE',  ( 0.000000000000000000, 1.000000000000000000, 0.000000000000000000 ) ) ;
#7619 = VERTEX_POINT ( 'NONE', #1704 ) ;
#7620 = CARTESIAN_POINT ( 'NONE',  ( 151.9741924115233473, 20.79694577634646535, -212.0849693193237897 ) ) ;
#7621 = ADVANCED_FACE ( 'NONE', ( #4026 ), #7538, .F. ) ;
#7622 = ORIENTED_EDGE ( 'NONE', *, *, #3719, .F. ) ;
#7623 = CARTESIAN_POINT ( 'NONE',  ( -122.2593324768321992, 30.00000000000000000, 168.2755348299905052 ) ) ;
#7624 = ORIENTED_EDGE ( 'NONE', *, *, #5432, .T. ) ;
#7625 = VERTEX_POINT ( 'NONE', #11900 ) ;
#7626 = AXIS2_PLACEMENT_3D ( 'NONE', #12075, #4941, #8951 ) ;
#7627 = DIRECTION ( 'NONE',  ( 0.6368676505102707219, 0.000000000000000000, 0.7709731485165535192 ) ) ;
#7628 = CARTESIAN_POINT ( 'NONE',  ( -229.6889200636375108, -1.000000000000000000, 11.95826074310140008 ) ) ;
#7629 = DIRECTION ( 'NONE',  ( 0.6368676505102716101, 0.000000000000000000, 0.7709731485165527420 ) ) ;
#7630 = ADVANCED_FACE ( 'NONE', ( #2748 ), #96, .F. ) ;
#7631 = CYLINDRICAL_SURFACE ( 'NONE', #3495, 5.500000000000005329 ) ;
#7632 = VECTOR ( 'NONE', #8323, 1000.000000000000000 ) ;
#7633 = AXIS2_PLACEMENT_3D ( 'NONE', #11255, #6195, #1196 ) ;
#7634 = VERTEX_POINT ( 'NONE', #1774 ) ;
#7635 = AXIS2_PLACEMENT_3D ( 'NONE', #5490, #9551, #2806 ) ;
#7636 = CARTESIAN_POINT ( 'NONE',  ( 0.000000000000000000, 0.000000000000000000, 0.000000000000000000 ) ) ;
#7637 = ORIENTED_EDGE ( 'NONE', *, *, #8326, .T. ) ;
#7638 = CARTESIAN_POINT ( 'NONE',  ( -242.7734209817145370, 7.097132676516893390, -9.364576599533018353 ) ) ;
#7639 = DIRECTION ( 'NONE',  ( -1.000000000000000000, 0.000000000000000000, 0.000000000000000000 ) ) ;
#7640 = CONICAL_SURFACE ( 'NONE', #11274, 249.7999999999999829, 0.7853981633975309906 ) ;
#7641 = FACE_OUTER_BOUND ( 'NONE', #9049, .T. ) ;
#7642 = CARTESIAN_POINT ( 'NONE',  ( -294.1869546181095529, -30.00000000000000000, -31.92980917095498938 ) ) ;
#7643 = CARTESIAN_POINT ( 'NONE',  ( 0.000000000000000000, 19.00000000000000000, 208.0000000000000000 ) ) ;
#7644 = CARTESIAN_POINT ( 'NONE',  ( -240.9194688706963063, -4.677296209585168008, -10.77948277536260591 ) ) ;
#7645 = CIRCLE ( 'NONE', #9770, 5.500000000000005329 ) ;
#7646 = CARTESIAN_POINT ( 'NONE',  ( -245.6532195756332442, -9.065612403241397388, 7.862145249027526539 ) ) ;
#7647 = DIRECTION ( 'NONE',  ( 0.6368676505102707219, 0.000000000000000000, 0.7709731485165535192 ) ) ;
#7648 = ITEM_DEFINED_TRANSFORMATION ( 'NONE', 'NONE', #3142,  #805 ) ;
#7649 = CARTESIAN_POINT ( 'NONE',  ( -229.7396222156540944, 4.940198752275430927, 10.94224479212417300 ) ) ;
#7650 = VECTOR ( 'NONE', #5562, 1000.000000000000000 ) ;
#7651 = ORIENTED_EDGE ( 'NONE', *, *, #738, .F. ) ;
#7652 = ORIENTED_EDGE ( 'NONE', *, *, #1769, .F. ) ;
#7653 = FACE_OUTER_BOUND ( 'NONE', #8754, .T. ) ;
#7654 = ORIENTED_EDGE ( 'NONE', *, *, #107, .T. ) ;
#7655 = CARTESIAN_POINT ( 'NONE',  ( 207.6469600138280498, 19.96883746145561389, 159.3024069661363740 ) ) ;
#7656 = CARTESIAN_POINT ( 'NONE',  ( 0.000000000000000000, 29.00000000000000000, 208.0000000000000000 ) ) ;
#7657 = DIRECTION ( 'NONE',  ( 0.000000000000000000, 0.000000000000000000, -1.000000000000000000 ) ) ;
#7658 =( REPRESENTATION_RELATIONSHIP ('NONE','NONE', #12019, #5191 ) REPRESENTATION_RELATIONSHIP_WITH_TRANSFORMATION ( #6072 )SHAPE_REPRESENTATION_RELATIONSHIP( ) );
#7659 = DIRECTION ( 'NONE',  ( 0.000000000000000000, 1.000000000000000000, 0.000000000000000000 ) ) ;
#7660 = EDGE_CURVE ( 'NONE', #8275, #6828, #5841, .T. ) ;
#7661 = CARTESIAN_POINT ( 'NONE',  ( -240.1208361041834962, -2.772967769359314882, 11.41810622433041900 ) ) ;
#7662 = ADVANCED_FACE ( 'NONE', ( #837 ), #2830, .F. ) ;
#7663 = DIRECTION ( 'NONE',  ( -0.000000000000000000, -1.000000000000000000, 0.000000000000000000 ) ) ;
#7664 = DIRECTION ( 'NONE',  ( 0.1736481776669273613, 0.000000000000000000, 0.9848077530122085754 ) ) ;
#7665 = CARTESIAN_POINT ( 'NONE',  ( -229.6996680450365318, -0.7764858098324382008, -11.75000000000000178 ) ) ;
#7666 = ITEM_DEFINED_TRANSFORMATION ( 'NONE', 'NONE', #825,  #805 ) ;
#7667 = CIRCLE ( 'NONE', #1929, 196.0000000000000000 ) ;
#7668 = CARTESIAN_POINT ( 'NONE',  ( -240.0092717900809873, -2.435426586977146535, -11.75368411293068682 ) ) ;
#7669 = CARTESIAN_POINT ( 'NONE',  ( -229.8082689465775559, -7.478642794604872357, 9.391993320510708898 ) ) ;
#7670 = ORIENTED_EDGE ( 'NONE', *, *, #10595, .F. ) ;
#7671 = ORIENTED_EDGE ( 'NONE', *, *, #2892, .T. ) ;
#7672 = PRODUCT_DEFINITION ( 'UNKNOWN', '', #9170, #8887 ) ;
#7673 = AXIS2_PLACEMENT_3D ( 'NONE', #10930, #5803, #3789 ) ;
#7674 = DIRECTION ( 'NONE',  ( -0.6368676505102708330, 0.000000000000000000, -0.7709731485165536302 ) ) ;
#7675 = CARTESIAN_POINT ( 'NONE',  ( 222.8706404512946904, -3.349349297028606731, 0.06602489298702547693 ) ) ;
#7676 = CARTESIAN_POINT ( 'NONE',  ( 259.6535381495593242, 20.55460285082940075, -34.20858920423904692 ) ) ;
#7677 = DIRECTION ( 'NONE',  ( -0.6368676505102689456, 0.000000000000000000, -0.7709731485165549625 ) ) ;
#7678 = DIRECTION ( 'NONE',  ( -0.9063077870366523792, 0.000000000000000000, 0.4226182617406942787 ) ) ;
#7679 = CARTESIAN_POINT ( 'NONE',  ( 0.000000000000000000, 30.00000000000000000, 208.0000000000000000 ) ) ;
#7680 = CARTESIAN_POINT ( 'NONE',  ( 240.1364042142066921, 2.243206690540103576, -2.686876444944948261 ) ) ;
#7681 = PRODUCT_DEFINITION_FORMATION_WITH_SPECIFIED_SOURCE ( 'ANY', '', #219, .NOT_KNOWN. ) ;
#7682 = EDGE_LOOP ( 'NONE', ( #6926, #4375 ) ) ;
#7683 = PLANE ( 'NONE',  #4334 ) ;
#7684 = DIRECTION ( 'NONE',  ( -0.6368676505102690566, 0.000000000000000000, -0.7709731485165549625 ) ) ;
#7685 = ORIENTED_EDGE ( 'NONE', *, *, #1723, .F. ) ;
#7686 = EDGE_LOOP ( 'NONE', ( #12011, #776, #9872, #6857 ) ) ;
#7687 = ADVANCED_FACE ( 'NONE', ( #106 ), #6480, .T. ) ;
#7688 = CIRCLE ( 'NONE', #3427, 3.000000000000000000 ) ;
#7689 = EDGE_CURVE ( 'NONE', #9991, #2838, #9298, .T. ) ;
#7690 = VERTEX_POINT ( 'NONE', #2227 ) ;
#7691 = CYLINDRICAL_SURFACE ( 'NONE', #1564, 4.000000000000000000 ) ;
#7692 = CARTESIAN_POINT ( 'NONE',  ( -246.7009519923207108, 9.473788075149697008, 6.950529152119087506 ) ) ;
#7693 = CARTESIAN_POINT ( 'NONE',  ( -122.2593324768321992, 19.00000000000000000, 162.7755348299905052 ) ) ;
#7694 = CARTESIAN_POINT ( 'NONE',  ( 83.95474316006190918, 20.08915143290042948, -247.2466869557860036 ) ) ;
#7695 = DIRECTION ( 'NONE',  ( 0.000000000000000000, 1.000000000000000000, 0.000000000000000000 ) ) ;
#7696 = FILL_AREA_STYLE_COLOUR ( '', #2190 ) ;
#7697 = CONTEXT_DEPENDENT_SHAPE_REPRESENTATION ( #5247, #11216 ) ;
#7698 = ORIENTED_EDGE ( 'NONE', *, *, #6171, .F. ) ;
#7699 = CARTESIAN_POINT ( 'NONE',  ( 135.8846079354933352, -30.00000000000000000, -256.1940150085812888 ) ) ;
#7700 = EDGE_LOOP ( 'NONE', ( #11827, #10871, #8857, #401 ) ) ;
#7701 = CARTESIAN_POINT ( 'NONE',  ( -240.4180123852993916, 3.650278635439865305, -11.17777342488509440 ) ) ;
#7702 = VERTEX_POINT ( 'NONE', #12367 ) ;
#7703 = CIRCLE ( 'NONE', #1959, 2.475000000000000089 ) ;
#7704 = EDGE_CURVE ( 'NONE', #552, #1965, #6898, .T. ) ;
#7705 = DIRECTION ( 'NONE',  ( -0.000000000000000000, -1.000000000000000000, 0.000000000000000000 ) ) ;
#7706 = FACE_BOUND ( 'NONE', #1581, .T. ) ;
#7707 = CARTESIAN_POINT ( 'NONE',  ( -249.7601711286370971, -11.14534860557855822, -4.601188512101209938 ) ) ;
#7708 = AXIS2_PLACEMENT_3D ( 'NONE', #414, #2597, #6686 ) ;
#7709 = CARTESIAN_POINT ( 'NONE',  ( 185.9653539490014111, -29.00000000000000000, 225.1241593668316625 ) ) ;
#7710 = PRODUCT_DEFINITION_SHAPE ( 'NONE', 'NONE',  #13145 ) ;
#7711 = DIRECTION ( 'NONE',  ( 0.000000000000000000, 0.7071067811865450192, 0.7071067811865500152 ) ) ;
#7712 = AXIS2_PLACEMENT_3D ( 'NONE', #11361, #2222, #6300 ) ;
#7713 = CARTESIAN_POINT ( 'NONE',  ( -197.8197553893909912, 30.00000000000000000, 57.77553482999130807 ) ) ;
#7714 = CIRCLE ( 'NONE', #5586, 5.499999999999998224 ) ;
#7715 = CARTESIAN_POINT ( 'NONE',  ( -230.0000037765768184, 12.00007008448874579, -0.1815857884241967868 ) ) ;
#7716 = ITEM_DEFINED_TRANSFORMATION ( 'NONE', 'NONE', #10653,  #805 ) ;
#7717 = ORIENTED_EDGE ( 'NONE', *, *, #7741, .F. ) ;
#7718 = ORIENTED_EDGE ( 'NONE', *, *, #6859, .F. ) ;
#7719 = CARTESIAN_POINT ( 'NONE',  ( -249.7981860224685704, -11.73141662623283565, -0.7273454552846162491 ) ) ;
#7720 = ORIENTED_EDGE ( 'NONE', *, *, #864, .F. ) ;
#7721 = VECTOR ( 'NONE', #6085, 1000.000000000000000 ) ;
#7722 = CARTESIAN_POINT ( 'NONE',  ( -261.3381329044966606, 20.55460285096646089, -17.10461161606123426 ) ) ;
#7723 = CARTESIAN_POINT ( 'NONE',  ( 71.82423009839129691, 19.40000000000000213, 192.2354503650404922 ) ) ;
#7724 = CARTESIAN_POINT ( 'NONE',  ( 227.3999999999999773, 4.550331206106116078, 2.508881407069060376 ) ) ;
#7725 =( GEOMETRIC_REPRESENTATION_CONTEXT ( 3 ) GLOBAL_UNCERTAINTY_ASSIGNED_CONTEXT ( ( #12114 ) ) GLOBAL_UNIT_ASSIGNED_CONTEXT ( ( #4426, #6516, #4492 ) ) REPRESENTATION_CONTEXT ( 'NONE', 'WORKASPACE' ) );
#7726 = CARTESIAN_POINT ( 'NONE',  ( 0.000000000000000000, 18.00000000000000000, 0.000000000000000000 ) ) ;
#7727 = CARTESIAN_POINT ( 'NONE',  ( -240.4848270099804779, 3.809198625029032836, 11.37937944661116596 ) ) ;
#7728 = FACE_OUTER_BOUND ( 'NONE', #4679, .T. ) ;
#7729 = CARTESIAN_POINT ( 'NONE',  ( 10.83189848055877036, -138.4705547276867321, -40.42519547187224305 ) ) ;
#7730 = VECTOR ( 'NONE', #6901, 1000.000000000000114 ) ;
#7731 = CARTESIAN_POINT ( 'NONE',  ( -229.8013896584316171, -6.844199613598257237, -9.558601023545847397 ) ) ;
#7732 = AXIS2_PLACEMENT_3D ( 'NONE', #2439, #6776, #9693 ) ;
#7733 = CONTEXT_DEPENDENT_SHAPE_REPRESENTATION ( #9262, #2812 ) ;
#7734 = CONICAL_SURFACE ( 'NONE', #10926, 5.500000000000015099, 0.7853981633974461696 ) ;
#7735 = CARTESIAN_POINT ( 'NONE',  ( -249.7931653178112299, 11.67801679592136033, 1.333825769639327197 ) ) ;
#7736 = CARTESIAN_POINT ( 'NONE',  ( -136.1890905123932498, -25.00000000000000000, 208.4551069784743049 ) ) ;
#7737 = CARTESIAN_POINT ( 'NONE',  ( -229.8466860526774838, -8.576889844641714333, -8.400978990607617547 ) ) ;
#7738 = EDGE_LOOP ( 'NONE', ( #12149, #9553, #9506, #12431 ) ) ;
#7739 = EDGE_CURVE ( 'NONE', #12258, #7200, #2209, .T. ) ;
#7740 = ORIENTED_EDGE ( 'NONE', *, *, #3019, .T. ) ;
#7741 = EDGE_CURVE ( 'NONE', #3428, #3301, #3907, .T. ) ;
#7742 = CARTESIAN_POINT ( 'NONE',  ( 227.3999999999999773, -4.447920636657316074, 2.686261716586446635 ) ) ;
#7743 = CARTESIAN_POINT ( 'NONE',  ( 0.000000000000000000, -2.926905849962176352E-14, 0.000000000000000000 ) ) ;
#7744 = PRODUCT_DEFINITION_SHAPE ( 'NONE', 'NONE',  #13062 ) ;
#7745 = AXIS2_PLACEMENT_3D ( 'NONE', #8347, #4267, #11545 ) ;
#7746 = CIRCLE ( 'NONE', #8189, 5.499999999999998224 ) ;
#7747 = CARTESIAN_POINT ( 'NONE',  ( -172.3268284098719789, 20.79694577634883856, 196.4640694352564765 ) ) ;
#7748 = CARTESIAN_POINT ( 'NONE',  ( 71.82423009839129691, 30.00000000000000000, 197.3354503650404865 ) ) ;
#7749 = DIRECTION ( 'NONE',  ( 0.9396926207859115365, 0.000000000000000000, -0.3420201433256601642 ) ) ;
#7750 = CARTESIAN_POINT ( 'NONE',  ( 197.8197553893915028, 30.00000000000000000, -64.27553482998990830 ) ) ;
#7751 = DIRECTION ( 'NONE',  ( 0.000000000000000000, 0.000000000000000000, 1.000000000000000000 ) ) ;
#7752 = ORIENTED_EDGE ( 'NONE', *, *, #8978, .T. ) ;
#7753 = AXIS2_PLACEMENT_3D ( 'NONE', #8575, #6380, #10438 ) ;
#7754 = LINE ( 'NONE', #10753, #1893 ) ;
#7755 = VERTEX_POINT ( 'NONE', #3218 ) ;
#7756 = ORIENTED_EDGE ( 'NONE', *, *, #10963, .F. ) ;
#7757 = ADVANCED_FACE ( 'NONE', ( #12491 ), #4538, .F. ) ;
#7758 = CARTESIAN_POINT ( 'NONE',  ( 67.47543992452030182, 20.08915143297736350, 251.8100110699621439 ) ) ;
#7759 = ORIENTED_EDGE ( 'NONE', *, *, #4845, .T. ) ;
#7760 = CARTESIAN_POINT ( 'NONE',  ( 24.18668477630848557, -19.00000000000000000, -294.9245348571437262 ) ) ;
#7761 = DIRECTION ( 'NONE',  ( 0.000000000000000000, 0.000000000000000000, 1.000000000000000000 ) ) ;
#7762 = CARTESIAN_POINT ( 'NONE',  ( -115.4648407704221995, 20.08915143316778895, 234.1947771724274787 ) ) ;
#7763 = VECTOR ( 'NONE', #8065, 1000.000000000000000 ) ;
#7764 = DIRECTION ( 'NONE',  ( 0.000000000000000000, 1.000000000000000000, 0.000000000000000000 ) ) ;
#7765 = CARTESIAN_POINT ( 'NONE',  ( 122.2593324768334071, 30.00000000000000000, -168.2755348299895104 ) ) ;
#7766 = EDGE_CURVE ( 'NONE', #8820, #1725, #9027, .T. ) ;
#7767 = EDGE_CURVE ( 'NONE', #2492, #1001, #7298, .T. ) ;
#7768 = ORIENTED_EDGE ( 'NONE', *, *, #7381, .T. ) ;
#7769 = CARTESIAN_POINT ( 'NONE',  ( 235.4000000000000057, 0.000000000000000000, 0.000000000000000000 ) ) ;
#7770 = ORIENTED_EDGE ( 'NONE', *, *, #11589, .T. ) ;
#7771 = CARTESIAN_POINT ( 'NONE',  ( -243.1473425732729936, 7.439266815432667990, -9.095043743639278588 ) ) ;
#7772 = EDGE_LOOP ( 'NONE', ( #1625, #9630, #6385, #4211 ) ) ;
#7773 = CARTESIAN_POINT ( 'NONE',  ( 23.54981712579822073, -18.00000000000000000, -295.6955080056602583 ) ) ;
#7774 = DIRECTION ( 'NONE',  ( -0.000000000000000000, -1.000000000000000000, 0.000000000000000000 ) ) ;
#7775 = LINE ( 'NONE', #10977, #3381 ) ;
#7776 = DIRECTION ( 'NONE',  ( 0.000000000000000000, -1.000000000000000000, 0.000000000000000000 ) ) ;
#7777 = CARTESIAN_POINT ( 'NONE',  ( -244.8348239361274352, -8.646460184833234308, 8.320981818661996599 ) ) ;
#7778 = CIRCLE ( 'NONE', #3092, 12.00000000000000000 ) ;
#7779 = EDGE_CURVE ( 'NONE', #3483, #8825, #6609, .T. ) ;
#7780 = DIRECTION ( 'NONE',  ( 0.000000000000000000, 0.9998057603070480415, -0.01970892327970899874 ) ) ;
#7781 = SHAPE_DEFINITION_REPRESENTATION ( #3697, #11156 ) ;
#7782 =( REPRESENTATION_RELATIONSHIP ('NONE','NONE', #12019, #182 ) REPRESENTATION_RELATIONSHIP_WITH_TRANSFORMATION ( #6219 )SHAPE_REPRESENTATION_RELATIONSHIP( ) );
#7783 = ORIENTED_EDGE ( 'NONE', *, *, #5209, .F. ) ;
#7784 = CARTESIAN_POINT ( 'NONE',  ( -229.9928007510749524, 11.86142183433858577, -1.856684144637750666 ) ) ;
#7785 = ORIENTED_EDGE ( 'NONE', *, *, #8459, .T. ) ;
#7786 = ADVANCED_FACE ( 'NONE', ( #4480 ), #3484, .F. ) ;
#7787 = DIRECTION ( 'NONE',  ( -0.000000000000000000, -1.000000000000000000, 0.000000000000000000 ) ) ;
#7788 = EDGE_LOOP ( 'NONE', ( #1122, #5244, #7371, #11748 ) ) ;
#7789 = CARTESIAN_POINT ( 'NONE',  ( 234.8993005740659044, 20.55460285055905700, 115.8123742914903289 ) ) ;
#7790 = CARTESIAN_POINT ( 'NONE',  ( 197.8197553893920144, 29.00000000000000000, 69.77553482998851564 ) ) ;
#7791 = DIRECTION ( 'NONE',  ( 0.000000000000000000, 1.000000000000000000, 0.000000000000000000 ) ) ;
#7792 = CARTESIAN_POINT ( 'NONE',  ( -247.5777789808319369, -9.724056904989312855, -6.595774162712118915 ) ) ;
#7793 = CARTESIAN_POINT ( 'NONE',  ( -241.0259582382434473, 4.889855348911388511, 10.95996151967449705 ) ) ;
#7794 = CYLINDRICAL_SURFACE ( 'NONE', #260, 3.499999999999964917 ) ;
#7795 = DIRECTION ( 'NONE',  ( -0.2154914511802816790, 0.5538822189107470706, -0.8042250444015801580 ) ) ;
#7796 = CARTESIAN_POINT ( 'NONE',  ( -229.9961401285962381, -11.67517309355853783, -1.533254299341943128 ) ) ;
#7797 = CONTEXT_DEPENDENT_SHAPE_REPRESENTATION ( #8582, #11020 ) ;
#7798 = CARTESIAN_POINT ( 'NONE',  ( -249.7845036514871424, 11.60839712335144114, -1.818694302537078977 ) ) ;
#7799 = CARTESIAN_POINT ( 'NONE',  ( -242.2196200855140091, -6.532801875576883965, -10.06598912834544635 ) ) ;
#7800 = CARTESIAN_POINT ( 'NONE',  ( -229.7113347995026231, -3.365903791379974752, -11.51977029171405853 ) ) ;
#7801 = VERTEX_POINT ( 'NONE', #7560 ) ;
#7802 = ORIENTED_EDGE ( 'NONE', *, *, #252, .F. ) ;
#7803 = LINE ( 'NONE', #2860, #10319 ) ;
#7804 = LINE ( 'NONE', #2665, #7952 ) ;
#7805 = CARTESIAN_POINT ( 'NONE',  ( -159.0697709836499882, 20.79694577635847352, 207.3438552937170130 ) ) ;
#7806 = FACE_OUTER_BOUND ( 'NONE', #8790, .T. ) ;
#7807 = DIRECTION ( 'NONE',  ( -0.3420201433256601642, 0.000000000000000000, -0.9396926207859115365 ) ) ;
#7808 = CARTESIAN_POINT ( 'NONE',  ( -24.18668477630637526, -19.00000000000000000, 294.9245348571438967 ) ) ;
#7809 = ADVANCED_FACE ( 'NONE', ( #10620, #8498 ), #7683, .F. ) ;
#7810 = ORIENTED_EDGE ( 'NONE', *, *, #10265, .F. ) ;
#7811 = CARTESIAN_POINT ( 'NONE',  ( -239.6569666445801374, -1.960938217768839920, 11.83870082047461914 ) ) ;
#7812 = ORIENTED_EDGE ( 'NONE', *, *, #2578, .F. ) ;
#7813 = ORIENTED_EDGE ( 'NONE', *, *, #4064, .T. ) ;
#7814 = CARTESIAN_POINT ( 'NONE',  ( 239.7985776503645354, -1.848645179573700004, 2.971954070984049956 ) ) ;
#7815 = ORIENTED_EDGE ( 'NONE', *, *, #5256, .T. ) ;
#7816 = PRODUCT_DEFINITION_SHAPE ( 'NONE', 'NONE',  #13153 ) ;
#7817 = DIRECTION ( 'NONE',  ( 0.000000000000000000, -1.000000000000000000, 0.000000000000000000 ) ) ;
#7818 = CIRCLE ( 'NONE', #5481, 6.500000000000005329 ) ;
#7819 = FACE_BOUND ( 'NONE', #4681, .T. ) ;
#7820 = CARTESIAN_POINT ( 'NONE',  ( 139.1326329530957082, -19.40000000000000213, -252.2620519511468729 ) ) ;
#7821 = SHAPE_REPRESENTATION_RELATIONSHIP ( 'NONE' , 'NONE' ,  #11671, #6344 ) ;
#7822 = CARTESIAN_POINT ( 'NONE',  ( -247.5777789797446928, 9.724056904727886419, 6.595774163021543401 ) ) ;
#7823 = ADVANCED_FACE ( 'NONE', ( #5554 ), #2625, .T. ) ;
#7824 = ADVANCED_FACE ( 'NONE', ( #563 ), #3413, .F. ) ;
#7825 = ORIENTED_EDGE ( 'NONE', *, *, #6723, .F. ) ;
#7826 = DIRECTION ( 'NONE',  ( 0.6368676505102716101, 0.000000000000000000, 0.7709731485165527420 ) ) ;
#7828 = ORIENTED_EDGE ( 'NONE', *, *, #446, .F. ) ;
#7827 = AXIS2_PLACEMENT_3D ( 'NONE', #11363, #5084, #9429 ) ;
#7829 = CARTESIAN_POINT ( 'NONE',  ( -246.5049976578405051, 9.406509142110611066, -7.041467212631606465 ) ) ;
#7830 = ORIENTED_EDGE ( 'NONE', *, *, #2467, .T. ) ;
#7831 = EDGE_CURVE ( 'NONE', #1100, #6702, #3263, .T. ) ;
#7832 = DIRECTION ( 'NONE',  ( 0.000000000000000000, 0.000000000000000000, 1.000000000000000000 ) ) ;
#7833 = CARTESIAN_POINT ( 'NONE',  ( 27.68945685411497593, -30.00000000000000000, -290.6841825403026291 ) ) ;
#7834 = DIRECTION ( 'NONE',  ( 0.000000000000000000, 1.000000000000000000, 0.000000000000000000 ) ) ;
#7835 = VECTOR ( 'NONE', #9253, 1000.000000000000000 ) ;
#7836 = AXIS2_PLACEMENT_3D ( 'NONE', #5881, #3803, #12012 ) ;
#7837 = DIRECTION ( 'NONE',  ( 0.000000000000000000, 0.000000000000000000, -1.000000000000000000 ) ) ;
#7838 = VECTOR ( 'NONE', #3062, 1000.000000000000000 ) ;
#7839 = AXIS2_PLACEMENT_3D ( 'NONE', #7150, #10136, #6286 ) ;
#7840 = CARTESIAN_POINT ( 'NONE',  ( -260.1353576186481860, 20.08915143297736705, 17.05322212017742345 ) ) ;
#7841 = CARTESIAN_POINT ( 'NONE',  ( -244.7207088053502275, -8.581273367803877505, 8.388577729903433422 ) ) ;
#7842 = CARTESIAN_POINT ( 'NONE',  ( -239.0463147780496058, 1.265540212841881118, -11.93307915084255555 ) ) ;
#7843 = ITEM_DEFINED_TRANSFORMATION ( 'NONE', 'NONE', #10600,  #805 ) ;
#7844 = VERTEX_POINT ( 'NONE', #8476 ) ;
#7845 = CARTESIAN_POINT ( 'NONE',  ( -238.7984611738133651, -0.6745683551878548512, -11.73164972064059697 ) ) ;
#7846 = CONTEXT_DEPENDENT_SHAPE_REPRESENTATION ( #6127, #10679 ) ;
#7847 = EDGE_LOOP ( 'NONE', ( #5742, #3072, #8320, #10754 ) ) ;
#7848 = PRODUCT_DEFINITION_SHAPE ( 'NONE', 'NONE',  #13076 ) ;
#7849 = EDGE_LOOP ( 'NONE', ( #4304, #642, #9850, #10500 ) ) ;
#7850 = AXIS2_PLACEMENT_3D ( 'NONE', #9060, #11187, #2054 ) ;
#7851 = CARTESIAN_POINT ( 'NONE',  ( -248.9866437208148682, -10.23506904034385201, -5.772678315709418584 ) ) ;
#7852 = ORIENTED_EDGE ( 'NONE', *, *, #11514, .F. ) ;
#7853 = ADVANCED_FACE ( 'NONE', ( #11275 ), #6050, .F. ) ;
#7854 = CIRCLE ( 'NONE', #2103, 250.1999999999999602 ) ;
#7855 = CARTESIAN_POINT ( 'NONE',  ( 252.9796497720284094, 20.55460285130353881, -67.76049180262273808 ) ) ;
#7856 = EDGE_CURVE ( 'NONE', #8770, #6308, #9277, .T. ) ;
#7857 = DIRECTION ( 'NONE',  ( 0.000000000000000000, 1.000000000000000000, 0.000000000000000000 ) ) ;
#7858 = CARTESIAN_POINT ( 'NONE',  ( 122.2593324768346008, 18.00000000000000000, 174.7755348299889988 ) ) ;
#7859 = CIRCLE ( 'NONE', #11269, 5.500000000000005329 ) ;
#7860 = FACE_OUTER_BOUND ( 'NONE', #7738, .T. ) ;
#7861 = CARTESIAN_POINT ( 'NONE',  ( -242.0646888581063081, 6.354939415246917633, 10.17926273054569641 ) ) ;
#7862 = CARTESIAN_POINT ( 'NONE',  ( 0.000000000000000000, 11.79660968244690089, 0.000000000000000000 ) ) ;
#7863 = CARTESIAN_POINT ( 'NONE',  ( -7.267391899529818566, -138.4705547276867321, -41.21542755584199114 ) ) ;
#7864 = CARTESIAN_POINT ( 'NONE',  ( 229.9934143309166075, 3.039192421457848958, 1.750862794997881666 ) ) ;
#7865 = CARTESIAN_POINT ( 'NONE',  ( -249.7006323033828039, 11.24927497855769687, -3.394647652268084403 ) ) ;
#7866 = CARTESIAN_POINT ( 'NONE',  ( -249.7118339206215012, -9.997999799959989886, -6.636264009214830395 ) ) ;
#7867 = CARTESIAN_POINT ( 'NONE',  ( -229.9297054377521761, -10.57472760585867100, -5.721117632547625398 ) ) ;
#7868 = ORIENTED_EDGE ( 'NONE', *, *, #11443, .F. ) ;
#7869 = ORIENTED_EDGE ( 'NONE', *, *, #2754, .T. ) ;
#7870 = VECTOR ( 'NONE', #2265, 1000.000000000000000 ) ;
#7871 = DIRECTION ( 'NONE',  ( 1.000000000000000000, 0.000000000000000000, 0.000000000000000000 ) ) ;
#7872 = EDGE_CURVE ( 'NONE', #7994, #6551, #3194, .T. ) ;
#7873 = CARTESIAN_POINT ( 'NONE',  ( 11.00000000000000000, 0.000000000000000000, 250.0000000000000000 ) ) ;
#7874 = VECTOR ( 'NONE', #2306, 1000.000000000000000 ) ;
#7875 = CARTESIAN_POINT ( 'NONE',  ( 130.9697226058085846, 20.55460285117392516, 226.7975291051602937 ) ) ;
#7876 = CARTESIAN_POINT ( 'NONE',  ( -240.1208361041844910, -2.772967769359084844, -11.41810622433049893 ) ) ;
#7877 = DIRECTION ( 'NONE',  ( 0.7660444431189835646, 0.000000000000000000, -0.6427876096865327016 ) ) ;
#7878 = DIRECTION ( 'NONE',  ( 0.5469441386039890496, 0.000000000000000000, -0.8371691043312220470 ) ) ;
#7879 = FACE_OUTER_BOUND ( 'NONE', #3233, .T. ) ;
#7880 = EDGE_LOOP ( 'NONE', ( #4362, #11015, #8500, #6961 ) ) ;
#7881 = AXIS2_PLACEMENT_3D ( 'NONE', #3729, #4791, #9718 ) ;
#7882 = CARTESIAN_POINT ( 'NONE',  ( -233.0000000000000000, -1.000000000000000000, -12.50000000000000000 ) ) ;
#7883 = ORIENTED_EDGE ( 'NONE', *, *, #12469, .F. ) ;
#7884 = ORIENTED_EDGE ( 'NONE', *, *, #3916, .F. ) ;
#7885 = CARTESIAN_POINT ( 'NONE',  ( 240.1364042142084259, -2.243206690542109971, 2.686876444943266051 ) ) ;
#7886 = VERTEX_POINT ( 'NONE', #6142 ) ;
#7887 = AXIS2_PLACEMENT_3D ( 'NONE', #2406, #10542, #8546 ) ;
#7888 =( REPRESENTATION_RELATIONSHIP ('NONE','NONE', #12019, #5191 ) REPRESENTATION_RELATIONSHIP_WITH_TRANSFORMATION ( #11066 )SHAPE_REPRESENTATION_RELATIONSHIP( ) );
#7889 = CARTESIAN_POINT ( 'NONE',  ( -185.9653539489998195, -30.00000000000000000, -225.1241593668329699 ) ) ;
#7890 = DIRECTION ( 'NONE',  ( 0.000000000000000000, 0.000000000000000000, 1.000000000000000000 ) ) ;
#7891 = CARTESIAN_POINT ( 'NONE',  ( 0.000000000000000000, 2.772967769358929857, 0.000000000000000000 ) ) ;
#7892 = DIRECTION ( 'NONE',  ( 0.4503334343941555740, 0.7071067811865490160, 0.5451603414287971017 ) ) ;
#7893 = LINE ( 'NONE', #4756, #5597 ) ;
#7894 = VERTEX_POINT ( 'NONE', #7276 ) ;
#7895 = DIRECTION ( 'NONE',  ( 0.000000000000000000, 1.000000000000000000, 0.000000000000000000 ) ) ;
#7896 = EDGE_LOOP ( 'NONE', ( #126, #8373, #12350, #9892 ) ) ;
#7897 = CARTESIAN_POINT ( 'NONE',  ( -239.4550142662953078, 1.775421008909468634, 11.61532944475347584 ) ) ;
#7898 = EDGE_LOOP ( 'NONE', ( #12387, #2115, #11802, #3718 ) ) ;
#7899 = VECTOR ( 'NONE', #3636, 1000.000000000000000 ) ;
#7900 = AXIS2_PLACEMENT_3D ( 'NONE', #12926, #10995, #4058 ) ;
#7901 = EDGE_CURVE ( 'NONE', #5790, #11150, #1366, .T. ) ;
#7902 = EDGE_CURVE ( 'NONE', #5226, #3016, #11799, .T. ) ;
#7903 = LINE ( 'NONE', #12041, #10212 ) ;
#7904 = CARTESIAN_POINT ( 'NONE',  ( 240.0821326536456581, 2.149019271550664634, 2.771577408253355301 ) ) ;
#7905 = CARTESIAN_POINT ( 'NONE',  ( 290.6841825403032544, -18.00000000000000000, 27.68945685411186730 ) ) ;
#7906 = DIRECTION ( 'NONE',  ( 0.000000000000000000, -1.000000000000000000, 0.000000000000000000 ) ) ;
#7907 = VECTOR ( 'NONE', #4168, 1000.000000000000114 ) ;
#7908 = DIRECTION ( 'NONE',  ( -1.000000000000000000, 0.000000000000000000, 0.000000000000000000 ) ) ;
#7909 = CARTESIAN_POINT ( 'NONE',  ( -241.4289589284794033, -5.524154699785203348, 10.65313710557979299 ) ) ;
#7910 = CARTESIAN_POINT ( 'NONE',  ( 260.5542428351129729, 20.08915143297737416, -17.05314194230804858 ) ) ;
#7911 = CARTESIAN_POINT ( 'NONE',  ( -238.7879693988574559, 0.6590516398346927263, -11.98189593644098849 ) ) ;
#7912 = ORIENTED_EDGE ( 'NONE', *, *, #4257, .F. ) ;
#7913 = PRODUCT_RELATED_PRODUCT_CATEGORY ( 'part', '', ( #219 ) ) ;
#7914 = CARTESIAN_POINT ( 'NONE',  ( -239.1986675930642718, -1.476433817035277762, -11.65687006250814406 ) ) ;
#7915 = AXIS2_PLACEMENT_3D ( 'NONE', #4523, #8798, #12667 ) ;
#7916 = ITEM_DEFINED_TRANSFORMATION ( 'NONE', 'NONE', #10448,  #805 ) ;
#7917 = ORIENTED_EDGE ( 'NONE', *, *, #986, .T. ) ;
#7918 = ORIENTED_EDGE ( 'NONE', *, *, #9725, .F. ) ;
#7919 = CARTESIAN_POINT ( 'NONE',  ( -233.0000000000000000, 0.000000000000000000, -12.00000000000000000 ) ) ;
#7920 = ORIENTED_EDGE ( 'NONE', *, *, #3621, .F. ) ;
#7921 = CARTESIAN_POINT ( 'NONE',  ( 84.20717312394452847, 20.55460285104429019, 247.9906035367661161 ) ) ;
#7922 = CARTESIAN_POINT ( 'NONE',  ( -248.8841473305337217, 9.947364712431371103, -6.711964937433803513 ) ) ;
#7923 = FACE_OUTER_BOUND ( 'NONE', #4662, .T. ) ;
#7924 = PRODUCT_DEFINITION_SHAPE ( 'NONE', 'NONE',  #13169 ) ;
#7925 = AXIS2_PLACEMENT_3D ( 'NONE', #7748, #4737, #10677 ) ;
#7926 = LINE ( 'NONE', #6933, #8671 ) ;
#7927 = VECTOR ( 'NONE', #4301, 1000.000000000000114 ) ;
#7928 = DIRECTION ( 'NONE',  ( 0.000000000000000000, 0.000000000000000000, -1.000000000000000000 ) ) ;
#7929 = FILL_AREA_STYLE ('',( #9999 ) ) ;
#7930 = DIRECTION ( 'NONE',  ( 0.4162975160791038687, 0.5538822189107471816, -0.7210484489137158892 ) ) ;
#7931 = EDGE_CURVE ( 'NONE', #10501, #6584, #305, .T. ) ;
#7932 = CARTESIAN_POINT ( 'NONE',  ( 226.7234983661818717, 3.822755691033211001, -0.07535703595917098152 ) ) ;
#7933 = CONTEXT_DEPENDENT_SHAPE_REPRESENTATION ( #12660, #10798 ) ;
#7934 = ADVANCED_FACE ( 'NONE', ( #7343 ), #3054, .F. ) ;
#7935 = PRODUCT_DEFINITION_SHAPE ( 'NONE', 'NONE',  #13159 ) ;
#7936 = CIRCLE ( 'NONE', #11778, 6.500000000000026645 ) ;
#7937 = DIRECTION ( 'NONE',  ( 1.000000000000000000, 0.000000000000000000, 0.000000000000000000 ) ) ;
#7938 = AXIS2_PLACEMENT_3D ( 'NONE', #6182, #10235, #12308 ) ;
#7939 = ORIENTED_EDGE ( 'NONE', *, *, #2228, .F. ) ;
#7940 = ORIENTED_EDGE ( 'NONE', *, *, #5957, .F. ) ;
#7941 = DIRECTION ( 'NONE',  ( 0.000000000000000000, 0.000000000000000000, 1.000000000000000000 ) ) ;
#7942 = DIRECTION ( 'NONE',  ( 0.000000000000000000, 1.000000000000000000, 0.000000000000000000 ) ) ;
#7943 = CONICAL_SURFACE ( 'NONE', #3896, 6.500000000000005329, 0.7853981633974490562 ) ;
#7944 = VECTOR ( 'NONE', #3620, 1000.000000000000114 ) ;
#7945 = CARTESIAN_POINT ( 'NONE',  ( 115.5625104412701916, 20.79694577657783228, 234.3927740975209986 ) ) ;
#7946 = AXIS2_PLACEMENT_3D ( 'NONE', #2375, #4242, #5171 ) ;
#7947 = CARTESIAN_POINT ( 'NONE',  ( 122.2593324768346008, 30.00000000000000000, 168.2755348299889988 ) ) ;
#7948 = DIRECTION ( 'NONE',  ( -0.9659258262890663138, 0.000000000000000000, -0.2588190451025280669 ) ) ;
#7949 = CIRCLE ( 'NONE', #11145, 254.0000000000000000 ) ;
#7950 = CARTESIAN_POINT ( 'NONE',  ( -240.1208361041834962, -2.772967769359314882, 11.41810622433041900 ) ) ;
#7951 = EDGE_CURVE ( 'NONE', #9902, #644, #12853, .T. ) ;
#7952 = VECTOR ( 'NONE', #2604, 999.9999999999998863 ) ;
#7953 = ORIENTED_EDGE ( 'NONE', *, *, #5173, .T. ) ;
#7954 = DIRECTION ( 'NONE',  ( 0.000000000000000000, 1.000000000000000000, 0.000000000000000000 ) ) ;
#7955 = UNCERTAINTY_MEASURE_WITH_UNIT (LENGTH_MEASURE( 1.000000000000000082E-05 ), #11965, 'distance_accuracy_value', 'NONE');
#7956 = CARTESIAN_POINT ( 'NONE',  ( -239.4529136422323461, -1.782225441812128164, 11.86690534211290959 ) ) ;
#7957 = ORIENTED_EDGE ( 'NONE', *, *, #4626, .T. ) ;
#7958 = ORIENTED_EDGE ( 'NONE', *, *, #12873, .F. ) ;
#7959 = AXIS2_PLACEMENT_3D ( 'NONE', #1966, #6039, #2887 ) ;
#7960 = EDGE_CURVE ( 'NONE', #11915, #2131, #9877, .T. ) ;
#7961 = DIRECTION ( 'NONE',  ( 1.000000000000000000, 0.000000000000000000, 0.000000000000000000 ) ) ;
#7962 = ORIENTED_EDGE ( 'NONE', *, *, #3531, .F. ) ;
#7963 = CARTESIAN_POINT ( 'NONE',  ( -249.5790707038086396, 10.95560708660684668, 4.250203461109054004 ) ) ;
#7964 =( REPRESENTATION_RELATIONSHIP ('NONE','NONE', #12019, #182 ) REPRESENTATION_RELATIONSHIP_WITH_TRANSFORMATION ( #4976 )SHAPE_REPRESENTATION_RELATIONSHIP( ) );
#7965 = CARTESIAN_POINT ( 'NONE',  ( -159.3024069663917146, 19.96883746063718590, -207.6469600136618681 ) ) ;
#7966 = CARTESIAN_POINT ( 'NONE',  ( -239.7865846179036282, -2.059993154243251023, -11.82215868861702468 ) ) ;
#7967 = PRESENTATION_STYLE_ASSIGNMENT (( #11775 ) ) ;
#7968 = AXIS2_PLACEMENT_3D ( 'NONE', #8896, #9749, #8832 ) ;
#7969 = ORIENTED_EDGE ( 'NONE', *, *, #6119, .F. ) ;
#7970 = DIRECTION ( 'NONE',  ( 0.000000000000000000, 1.000000000000000000, 0.000000000000000000 ) ) ;
#7971 = ORIENTED_EDGE ( 'NONE', *, *, #6555, .F. ) ;
#7972 = CARTESIAN_POINT ( 'NONE',  ( -245.8522126038347437, 9.151584522525213927, -7.371153475566105229 ) ) ;
#7973 = ORIENTED_EDGE ( 'NONE', *, *, #4288, .F. ) ;
#7974 =( REPRESENTATION_RELATIONSHIP ('NONE','NONE', #12019, #182 ) REPRESENTATION_RELATIONSHIP_WITH_TRANSFORMATION ( #1148 )SHAPE_REPRESENTATION_RELATIONSHIP( ) );
#7975 = VECTOR ( 'NONE', #4755, 1000.000000000000000 ) ;
#7976 = TOROIDAL_SURFACE ( 'NONE', #1593, 238.4705882352940307, 2.000000000000000000 ) ;
#7977 = CARTESIAN_POINT ( 'NONE',  ( -159.3442861576697283, 0.000000000000000000, -192.8974817588416499 ) ) ;
#7978 = CARTESIAN_POINT ( 'NONE',  ( 240.3599429726978087, 2.697249171176622884, 2.233886006030612936 ) ) ;
#7979 = DIRECTION ( 'NONE',  ( -0.000000000000000000, -1.000000000000000000, 0.000000000000000000 ) ) ;
#7980 = DIRECTION ( 'NONE',  ( 0.000000000000000000, 0.000000000000000000, -1.000000000000000000 ) ) ;
#7981 = CARTESIAN_POINT ( 'NONE',  ( -178.2104428091931823, 20.08915143297737060, 190.2689011420768850 ) ) ;
#7982 = APPLICATION_CONTEXT ( 'automotive_design' ) ;
#7983 = CARTESIAN_POINT ( 'NONE',  ( -245.0420335985837426, -8.761757998096216582, 8.199751241974521321 ) ) ;
#7984 = CARTESIAN_POINT ( 'NONE',  ( -239.8728792811782284, 2.114429109107689442, -11.81232488172176964 ) ) ;
#7985 = UNCERTAINTY_MEASURE_WITH_UNIT (LENGTH_MEASURE( 1.000000000000000082E-05 ), #9750, 'distance_accuracy_value', 'NONE');
#7986 = ITEM_DEFINED_TRANSFORMATION ( 'NONE', 'NONE', #8491,  #805 ) ;
#7987 = ORIENTED_EDGE ( 'NONE', *, *, #10314, .T. ) ;
#7988 = CARTESIAN_POINT ( 'NONE',  ( 227.3999999999999773, 0.000000000000000000, 0.000000000000000000 ) ) ;
#7989 = EDGE_CURVE ( 'NONE', #366, #2919, #11340, .T. ) ;
#7990 = AXIS2_PLACEMENT_3D ( 'NONE', #12070, #9935, #680 ) ;
#7991 = VERTEX_POINT ( 'NONE', #4139 ) ;
#7992 = ORIENTED_EDGE ( 'NONE', *, *, #4667, .F. ) ;
#7993 = CARTESIAN_POINT ( 'NONE',  ( -249.7994463215831900, -11.74985191748826097, -0.3872576506385510542 ) ) ;
#7994 = VERTEX_POINT ( 'NONE', #6283 ) ;
#7995 = CARTESIAN_POINT ( 'NONE',  ( -252.9796497731091165, 20.55460285134058651, -67.76049180360037383 ) ) ;
#7996 = CARTESIAN_POINT ( 'NONE',  ( -248.1924789796937887, 9.852676062574365901, -6.850256174774278506 ) ) ;
#7997 = DIRECTION ( 'NONE',  ( -0.000000000000000000, -1.000000000000000000, 0.000000000000000000 ) ) ;
#7998 = DIRECTION ( 'NONE',  ( 0.000000000000000000, 0.000000000000000000, -1.000000000000000000 ) ) ;
#7999 = AXIS2_PLACEMENT_3D ( 'NONE', #6696, #9883, #3545 ) ;
#8000 = CARTESIAN_POINT ( 'NONE',  ( -245.8375576811710346, 9.148519945048249724, 7.766315672653775870 ) ) ;
#8001 = FACE_OUTER_BOUND ( 'NONE', #8855, .T. ) ;
#8002 = DIRECTION ( 'NONE',  ( 0.5351817705578463258, 0.5538822189107471816, 0.6378047977532591561 ) ) ;
#8003 = DIRECTION ( 'NONE',  ( -0.000000000000000000, -1.000000000000000000, 0.000000000000000000 ) ) ;
#8004 = EDGE_CURVE ( 'NONE', #4811, #4563, #2266, .T. ) ;
#8005 = ITEM_DEFINED_TRANSFORMATION ( 'NONE', 'NONE', #7673,  #805 ) ;
#8006 = VECTOR ( 'NONE', #11079, 1000.000000000000227 ) ;
#8007 = CARTESIAN_POINT ( 'NONE',  ( -229.7324912792606426, -4.597989431066022092, -11.09053087651768799 ) ) ;
#8008 = VERTEX_POINT ( 'NONE', #275 ) ;
#8009 = ORIENTED_EDGE ( 'NONE', *, *, #7009, .T. ) ;
#8010 = CARTESIAN_POINT ( 'NONE',  ( -250.0000000000000000, 1.469576158976823947E-15, 12.00000000000000000 ) ) ;
#8011 = CARTESIAN_POINT ( 'NONE',  ( 0.000000000000000000, -3.327561323230890267, 0.000000000000000000 ) ) ;
#8012 = ADVANCED_FACE ( 'NONE', ( #7205 ), #1375, .T. ) ;
#8013 = CARTESIAN_POINT ( 'NONE',  ( -240.1208361041844910, 2.772967769358964940, -11.41810622433052025 ) ) ;
#8014 = PLANE ( 'NONE',  #12826 ) ;
#8015 = CARTESIAN_POINT ( 'NONE',  ( 227.3999999999999773, -2.999417280921144346, 0.05912676983912736745 ) ) ;
#8016 = DIRECTION ( 'NONE',  ( -0.9961946980917461003, 0.000000000000000000, 0.08715574274765156004 ) ) ;
#8017 = DIRECTION ( 'NONE',  ( -0.000000000000000000, -1.000000000000000000, 0.000000000000000000 ) ) ;
#8018 = CONTEXT_DEPENDENT_SHAPE_REPRESENTATION ( #10252, #10197 ) ;
#8019 = ORIENTED_EDGE ( 'NONE', *, *, #11443, .T. ) ;
#8020 = CARTESIAN_POINT ( 'NONE',  ( 235.4000000000000057, 0.000000000000000000, 0.000000000000000000 ) ) ;
#8021 = DIRECTION ( 'NONE',  ( 0.000000000000000000, -1.000000000000000000, 0.000000000000000000 ) ) ;
#8022 = EDGE_LOOP ( 'NONE', ( #451, #1478 ) ) ;
#8023 = ORIENTED_EDGE ( 'NONE', *, *, #5236, .F. ) ;
#8024 = CYLINDRICAL_SURFACE ( 'NONE', #11478, 254.1999999999999886 ) ;
#8025 = CARTESIAN_POINT ( 'NONE',  ( 166.5596220099214406, -3.327561323230905366, 201.6321540179175997 ) ) ;
#8026 = ADVANCED_FACE ( 'NONE', ( #10472 ), #4346, .F. ) ;
#8027 = CARTESIAN_POINT ( 'NONE',  ( -249.1881502579952610, 10.41621036585313753, 5.437499737840824743 ) ) ;
#8028 = ADVANCED_FACE ( 'NONE', ( #4199 ), #4980, .T. ) ;
#8029 = CARTESIAN_POINT ( 'NONE',  ( -196.7513681794031868, 19.96883746182613706, -172.5787240283650590 ) ) ;
#8030 = CARTESIAN_POINT ( 'NONE',  ( -239.0539063777619617, -1.278329027785976457, -11.93171797770810727 ) ) ;
#8031 = CARTESIAN_POINT ( 'NONE',  ( -245.2557111572319855, 8.868800243844628284, 7.708496930521410384 ) ) ;
#8032 = ADVANCED_FACE ( 'NONE', ( #3390 ), #12014, .T. ) ;
#8033 = ORIENTED_EDGE ( 'NONE', *, *, #11828, .F. ) ;
#8034 = CARTESIAN_POINT ( 'NONE',  ( -239.1416205847678782, -1.396290246587958306, 11.66676345160061778 ) ) ;
#8035 = ORIENTED_EDGE ( 'NONE', *, *, #4879, .F. ) ;
#8036 = CARTESIAN_POINT ( 'NONE',  ( -246.6649006626714424, 9.461692665233195854, -6.966985663954976538 ) ) ;
#8037 = ORIENTED_EDGE ( 'NONE', *, *, #4669, .T. ) ;
#8038 = AXIS2_PLACEMENT_3D ( 'NONE', #11807, #10993, #10791 ) ;
#8039 =( REPRESENTATION_RELATIONSHIP ('NONE','NONE', #12019, #182 ) REPRESENTATION_RELATIONSHIP_WITH_TRANSFORMATION ( #5376 )SHAPE_REPRESENTATION_RELATIONSHIP( ) );
#8040 = FACE_OUTER_BOUND ( 'NONE', #4707, .T. ) ;
#8041 = EDGE_CURVE ( 'NONE', #8160, #7755, #10593, .T. ) ;
#8042 = DIRECTION ( 'NONE',  ( 0.000000000000000000, 1.000000000000000000, 0.000000000000000000 ) ) ;
#8043 = CARTESIAN_POINT ( 'NONE',  ( 239.4538130491550305, 1.465952997544165859, 3.178207852339172579 ) ) ;
#8044 = FACE_OUTER_BOUND ( 'NONE', #3109, .T. ) ;
#8045 = DIRECTION ( 'NONE',  ( 8.659560562354913137E-17, -0.7071067811865489050, 0.7071067811865460184 ) ) ;
#8046 = PRODUCT_DEFINITION_SHAPE ( 'NONE', 'NONE',  #13119 ) ;
#8047 = CARTESIAN_POINT ( 'NONE',  ( -241.3656950238382706, -5.430352949019471964, 10.70105707677801021 ) ) ;
#8048 = AXIS2_PLACEMENT_3D ( 'NONE', #7491, #10492, #4354 ) ;
#8049 = CARTESIAN_POINT ( 'NONE',  ( -239.4330564014918252, 1.762617352138328153, -11.86984317867509908 ) ) ;
#8050 = VERTEX_POINT ( 'NONE', #10908 ) ;
#8051 = DIRECTION ( 'NONE',  ( 0.000000000000000000, 0.000000000000000000, 1.000000000000000000 ) ) ;
#8052 = ORIENTED_EDGE ( 'NONE', *, *, #6441, .F. ) ;
#8053 = CARTESIAN_POINT ( 'NONE',  ( -249.1369139481503794, -10.36343465104323869, 5.538914405783208039 ) ) ;
#8054 = ORIENTED_EDGE ( 'NONE', *, *, #3655, .T. ) ;
#8055 = CIRCLE ( 'NONE', #8910, 240.3921568627444856 ) ;
#8056 = AXIS2_PLACEMENT_3D ( 'NONE', #11823, #9735, #3942 ) ;
#8057 = CARTESIAN_POINT ( 'NONE',  ( -226.3083638767344894, 20.79694577654763421, 130.6873781513949950 ) ) ;
#8058 = DIRECTION ( 'NONE',  ( 0.6368676505102708330, 0.000000000000000000, 0.7709731485165535192 ) ) ;
#8059 = DIRECTION ( 'NONE',  ( -0.000000000000000000, -1.000000000000000000, 0.000000000000000000 ) ) ;
#8060 = CARTESIAN_POINT ( 'NONE',  ( -242.5648157360982964, -6.889953639954495834, -9.518299936636116954 ) ) ;
#8061 = CARTESIAN_POINT ( 'NONE',  ( -249.1334134316369671, 9.986442412964869675, 6.653676027890797151 ) ) ;
#8062 = DIRECTION ( 'NONE',  ( 0.5000000000000101030, 0.000000000000000000, -0.8660254037844328234 ) ) ;
#8063 = CIRCLE ( 'NONE', #2309, 5.500000000000005329 ) ;
#8064 =( REPRESENTATION_RELATIONSHIP ('NONE','NONE', #12019, #5191 ) REPRESENTATION_RELATIONSHIP_WITH_TRANSFORMATION ( #5053 )SHAPE_REPRESENTATION_RELATIONSHIP( ) );
#8065 = DIRECTION ( 'NONE',  ( 8.659560562354963673E-17, 0.7071067811865450192, -0.7071067811865500152 ) ) ;
#8066 = CIRCLE ( 'NONE', #192, 6.499999999999999112 ) ;
#8067 = AXIS2_PLACEMENT_3D ( 'NONE', #4549, #5434, #8631 ) ;
#8068 = VECTOR ( 'NONE', #5964, 1000.000000000000114 ) ;
#8069 = CARTESIAN_POINT ( 'NONE',  ( 3.059167704270087661E-14, 25.50000000000000000, -249.7999999999999545 ) ) ;
#8070 = ORIENTED_EDGE ( 'NONE', *, *, #7381, .F. ) ;
#8071 = AXIS2_PLACEMENT_3D ( 'NONE', #11670, #9784, #1659 ) ;
#8072 = VERTEX_POINT ( 'NONE', #6608 ) ;
#8073 = VECTOR ( 'NONE', #2392, 1000.000000000000114 ) ;
#8074 = LINE ( 'NONE', #8010, #2234 ) ;
#8075 = DIRECTION ( 'NONE',  ( 0.000000000000000000, 0.000000000000000000, 1.000000000000000000 ) ) ;
#8076 = ADVANCED_FACE ( 'NONE', ( #6920, #11979, #10662, #783, #11912, #10979, #722, #5532, #2831, #1851, #1535, #2400, #6849, #5914, #2528 ), #4773, .F. ) ;
#8077 = EDGE_CURVE ( 'NONE', #6668, #2888, #2926, .T. ) ;
#8078 = CARTESIAN_POINT ( 'NONE',  ( -239.7946578092510208, 2.116498006234943219, -11.55893420607628563 ) ) ;
#8079 = AXIS2_PLACEMENT_3D ( 'NONE', #1389, #6461, #389 ) ;
#8080 = CARTESIAN_POINT ( 'NONE',  ( -159.6627199829248696, -25.00000000000000000, -193.2829683330999728 ) ) ;
#8081 = LINE ( 'NONE', #2997, #10271 ) ;
#8082 = AXIS2_PLACEMENT_3D ( 'NONE', #10083, #6153, #2871 ) ;
#8083 = CARTESIAN_POINT ( 'NONE',  ( 0.000000000000000000, 0.000000000000000000, 0.000000000000000000 ) ) ;
#8084 = CARTESIAN_POINT ( 'NONE',  ( -243.0711418327976219, -7.372150984762692261, 9.149572407291026721 ) ) ;
#8085 = ITEM_DEFINED_TRANSFORMATION ( 'NONE', 'NONE', #9742,  #805 ) ;
#8086 = ORIENTED_EDGE ( 'NONE', *, *, #8041, .T. ) ;
#8087 = PRODUCT_DEFINITION ( 'UNKNOWN', '', #13006, #11017 ) ;
#8088 = FACE_BOUND ( 'NONE', #12241, .T. ) ;
#8089 = CIRCLE ( 'NONE', #2960, 270.0000000000000000 ) ;
#8090 = CARTESIAN_POINT ( 'NONE',  ( -239.2621195213464205, -1.577673503500558017, 11.89604841280030278 ) ) ;
#8091 = ORIENTED_EDGE ( 'NONE', *, *, #624, .F. ) ;
#8092 = EDGE_LOOP ( 'NONE', ( #9199, #5476, #698, #9236 ) ) ;
#8093 = AXIS2_PLACEMENT_3D ( 'NONE', #3304, #6586, #5510 ) ;
#8094 = CARTESIAN_POINT ( 'NONE',  ( 197.8197553893920144, 19.00000000000000000, 58.77553482998850853 ) ) ;
#8095 = DIRECTION ( 'NONE',  ( -0.000000000000000000, -1.000000000000000000, 0.000000000000000000 ) ) ;
#8096 = DIRECTION ( 'NONE',  ( 0.000000000000000000, 0.000000000000000000, -1.000000000000000000 ) ) ;
#8097 =( REPRESENTATION_RELATIONSHIP ('NONE','NONE', #12019, #5191 ) REPRESENTATION_RELATIONSHIP_WITH_TRANSFORMATION ( #4130 )SHAPE_REPRESENTATION_RELATIONSHIP( ) );
#8098 = CARTESIAN_POINT ( 'NONE',  ( -1.008906662707803564E-12, 19.96883746059272724, 261.1558126970361400 ) ) ;
#8099 = AXIS2_PLACEMENT_3D ( 'NONE', #8998, #5799, #10857 ) ;
#8100 = CARTESIAN_POINT ( 'NONE',  ( 0.000000000000000000, 20.00000000000000000, 0.000000000000000000 ) ) ;
#8101 = CARTESIAN_POINT ( 'NONE',  ( -245.6948533149643765, 9.079155719285296300, 7.458842562578837487 ) ) ;
#8102 = ORIENTED_EDGE ( 'NONE', *, *, #4765, .F. ) ;
#8103 = FACE_OUTER_BOUND ( 'NONE', #9584, .T. ) ;
#8104 = EDGE_CURVE ( 'NONE', #9851, #237, #7246, .T. ) ;
#8105 = VERTEX_POINT ( 'NONE', #6051 ) ;
#8106 = EDGE_CURVE ( 'NONE', #8628, #4466, #4766, .T. ) ;
#8107 = CIRCLE ( 'NONE', #2762, 5.499999999999998224 ) ;
#8108 = CYLINDRICAL_SURFACE ( 'NONE', #1822, 245.7999999999999829 ) ;
#8109 = ORIENTED_EDGE ( 'NONE', *, *, #6060, .T. ) ;
#8110 = CARTESIAN_POINT ( 'NONE',  ( 226.7234983661818717, -3.822755691033211001, 0.07535703595917145337 ) ) ;
#8111 = DIRECTION ( 'NONE',  ( 0.000000000000000000, -1.000000000000000000, 0.000000000000000000 ) ) ;
#8112 = CARTESIAN_POINT ( 'NONE',  ( -210.0000000000000000, 19.40000000000000213, 0.000000000000000000 ) ) ;
#8113 = CARTESIAN_POINT ( 'NONE',  ( 0.000000000000000000, 21.99999999999995381, 0.000000000000000000 ) ) ;
#8114 = CARTESIAN_POINT ( 'NONE',  ( -122.2593324768359935, 29.00000000000000000, -173.7755348299880040 ) ) ;
#8115 = CARTESIAN_POINT ( 'NONE',  ( -196.0019244007917791, 20.08915143297737060, -171.8850263962756912 ) ) ;
#8116 = DIRECTION ( 'NONE',  ( 0.6368676505102689456, 0.000000000000000000, 0.7709731485165549625 ) ) ;
#8117 = CARTESIAN_POINT ( 'NONE',  ( -239.0387908900173386, 1.252775422852272058, -11.93442892142129885 ) ) ;
#8118 = VERTEX_POINT ( 'NONE', #11310 ) ;
#8119 = CARTESIAN_POINT ( 'NONE',  ( -238.7110724325390834, -0.02063703527941252586, -11.74998174837370968 ) ) ;
#8120 =( REPRESENTATION_RELATIONSHIP ('NONE','NONE', #12019, #5191 ) REPRESENTATION_RELATIONSHIP_WITH_TRANSFORMATION ( #745 )SHAPE_REPRESENTATION_RELATIONSHIP( ) );
#8121 = CARTESIAN_POINT ( 'NONE',  ( 197.8197553893915028, 19.00000000000000000, -69.77553482998990830 ) ) ;
#8122 = ORIENTED_EDGE ( 'NONE', *, *, #12656, .T. ) ;
#8123 = EDGE_CURVE ( 'NONE', #8455, #11555, #10106, .T. ) ;
#8124 = CIRCLE ( 'NONE', #6392, 10.00000000000000888 ) ;
#8125 = CARTESIAN_POINT ( 'NONE',  ( -249.6835501130389048, 11.19967427147338590, -3.553901703851193083 ) ) ;
#8126 = CARTESIAN_POINT ( 'NONE',  ( -243.6963328790141361, -7.900314958675253685, -9.035065364327605764 ) ) ;
#8127 = CARTESIAN_POINT ( 'NONE',  ( -122.2593324768359935, 19.00000000000000000, -168.2755348299880040 ) ) ;
#8128 = ORIENTED_EDGE ( 'NONE', *, *, #1992, .F. ) ;
#8129 = EDGE_CURVE ( 'NONE', #5922, #8469, #9885, .T. ) ;
#8130 = AXIS2_PLACEMENT_3D ( 'NONE', #8975, #11786, #10839 ) ;
#8131 = CARTESIAN_POINT ( 'NONE',  ( 234.3927740981229988, 20.79694577626769103, 115.5625104417014057 ) ) ;
#8132 = DIRECTION ( 'NONE',  ( 0.000000000000000000, 1.000000000000000000, 0.000000000000000000 ) ) ;
#8133 = DIRECTION ( 'NONE',  ( -0.000000000000000000, 1.000000000000000000, 0.000000000000000000 ) ) ;
#8134 = CARTESIAN_POINT ( 'NONE',  ( -246.7156022646194629, -9.478660876070511776, -6.943882023634849077 ) ) ;
#8135 = CARTESIAN_POINT ( 'NONE',  ( -122.2593324768321992, 18.00000000000000000, 161.7755348299905052 ) ) ;
#8136 = CARTESIAN_POINT ( 'NONE',  ( 234.3487510399341716, -2.474519256759935448, 0.04877958511727990831 ) ) ;
#8137 = FACE_OUTER_BOUND ( 'NONE', #1153, .T. ) ;
#8138 = DIRECTION ( 'NONE',  ( 0.8660254037844450359, 0.000000000000000000, -0.4999999999999888978 ) ) ;
#8139 = DIRECTION ( 'NONE',  ( 0.000000000000000000, -1.000000000000000000, 0.000000000000000000 ) ) ;
#8140 = CONTEXT_DEPENDENT_SHAPE_REPRESENTATION ( #8064, #5807 ) ;
#8141 = DIRECTION ( 'NONE',  ( -0.000000000000000000, -1.000000000000000000, 0.000000000000000000 ) ) ;
#8142 = EDGE_LOOP ( 'NONE', ( #9873, #3720, #11637, #7547 ) ) ;
#8143 = ORIENTED_EDGE ( 'NONE', *, *, #8106, .F. ) ;
#8144 = AXIS2_PLACEMENT_3D ( 'NONE', #12106, #4971, #178 ) ;
#8145 = CARTESIAN_POINT ( 'NONE',  ( -115.4648407707716018, 20.08915143296762906, -234.1947771733659920 ) ) ;
#8146 = CARTESIAN_POINT ( 'NONE',  ( 235.4000000000000057, 1.749660080537334128, -0.03449061573949074866 ) ) ;
#8147 = FACE_OUTER_BOUND ( 'NONE', #7299, .T. ) ;
#8148 = VECTOR ( 'NONE', #550, 1000.000000000000000 ) ;
#8149 = CARTESIAN_POINT ( 'NONE',  ( 0.000000000000000000, 30.00000000000000000, -208.0000000000000000 ) ) ;
#8150 = CYLINDRICAL_SURFACE ( 'NONE', #3673, 5.500000000000015099 ) ;
#8151 = CARTESIAN_POINT ( 'NONE',  ( 0.000000000000000000, 0.000000000000000000, 0.000000000000000000 ) ) ;
#8152 = AXIS2_PLACEMENT_3D ( 'NONE', #2667, #8748, #3675 ) ;
#8153 = CARTESIAN_POINT ( 'NONE',  ( -240.7240246252840734, -4.307698619074218804, 10.93373802362567027 ) ) ;
#8154 = CONTEXT_DEPENDENT_SHAPE_REPRESENTATION ( #5675, #3032 ) ;
#8155 = VERTEX_POINT ( 'NONE', #913 ) ;
#8156 = COLOUR_RGB ( '', 0.66274510, 0.83137255, 0.94901961) ;
#8157 = CARTESIAN_POINT ( 'NONE',  ( 229.9000000000000057, 0.000000000000000000, 0.000000000000000000 ) ) ;
#8158 = ADVANCED_FACE ( 'NONE', ( #979 ), #2896, .F. ) ;
#8159 = DIRECTION ( 'NONE',  ( 0.000000000000000000, 0.000000000000000000, -1.000000000000000000 ) ) ;
#8160 = VERTEX_POINT ( 'NONE', #11039 ) ;
#8161 = ORIENTED_EDGE ( 'NONE', *, *, #10480, .F. ) ;
#8162 = CARTESIAN_POINT ( 'NONE',  ( -185.9653539489998195, -30.00000000000000000, -225.1241593668329699 ) ) ;
#8163 = CARTESIAN_POINT ( 'NONE',  ( 0.000000000000000000, 19.00000000000000000, 208.0000000000000000 ) ) ;
#8164 = APPLICATION_CONTEXT ( 'automotive_design' ) ;
#8165 = PRODUCT_DEFINITION_SHAPE ( 'NONE', 'NONE',  #13134 ) ;
#8166 = CLOSED_SHELL ( 'NONE', ( #8987, #3837, #12633, #3213, #6413, #9499, #3135, #7472, #5706, #8963, #9613, #9246, #1654, #7457, #5867, #11002, #11990, #7128, #11442, #4555, #11922, #11919, #9707, #5268, #12724, #7687, #987, #2391, #7290, #2324, #11910, #2246, #5454, #11083, #3849, #12973, #12680, #2318, #4580, #4578, #9395, #6244 ) ) ;
#8167 = CARTESIAN_POINT ( 'NONE',  ( -159.3024069656823940, 19.96883745967399548, 207.6469600131863729 ) ) ;
#8168 = CARTESIAN_POINT ( 'NONE',  ( -239.5718914795530452, -1.891487842075796788, -11.85001484766223712 ) ) ;
#8169 = CARTESIAN_POINT ( 'NONE',  ( 0.000000000000000000, 0.000000000000000000, 0.000000000000000000 ) ) ;
#8170 = CARTESIAN_POINT ( 'NONE',  ( -242.3794917440154961, 6.695067658262285448, 9.656064787098769031 ) ) ;
#8171 = ORIENTED_EDGE ( 'NONE', *, *, #8004, .T. ) ;
#8172 = CARTESIAN_POINT ( 'NONE',  ( 258.6823826759384701, 20.79694577634646890, 34.05310945291972757 ) ) ;
#8173 = AXIS2_PLACEMENT_3D ( 'NONE', #1833, #4614, #3754 ) ;
#8174 = EDGE_CURVE ( 'NONE', #11763, #8424, #10732, .T. ) ;
#8175 = CIRCLE ( 'NONE', #2414, 251.2912898646364397 ) ;
#8176 = VERTEX_POINT ( 'NONE', #1978 ) ;
#8177 = AXIS2_PLACEMENT_3D ( 'NONE', #9736, #621, #10811 ) ;
#8178 = CARTESIAN_POINT ( 'NONE',  ( 224.4939760857161843, 6.051844909775672576, -0.1192985195352703198 ) ) ;
#8179 = ORIENTED_EDGE ( 'NONE', *, *, #4159, .F. ) ;
#8180 =( REPRESENTATION_RELATIONSHIP ('NONE','NONE', #12019, #5191 ) REPRESENTATION_RELATIONSHIP_WITH_TRANSFORMATION ( #9069 )SHAPE_REPRESENTATION_RELATIONSHIP( ) );
#8181 = LINE ( 'NONE', #8110, #7907 ) ;
#8182 = LINE ( 'NONE', #11035, #1051 ) ;
#8183 = EDGE_CURVE ( 'NONE', #10082, #12948, #1913, .T. ) ;
#8184 = DIRECTION ( 'NONE',  ( 0.000000000000000000, 0.9998057603070481525, -0.01970892327970899874 ) ) ;
#8185 = AXIS2_PLACEMENT_3D ( 'NONE', #8307, #231, #6238 ) ;
#8186 = EDGE_CURVE ( 'NONE', #1703, #4809, #10954, .T. ) ;
#8187 = DIRECTION ( 'NONE',  ( 0.4503334343941581830, -0.7071067811865450192, 0.5451603414288000993 ) ) ;
#8188 = CARTESIAN_POINT ( 'NONE',  ( -122.2593324768321992, 30.00000000000000000, 173.7755348299905052 ) ) ;
#8189 = AXIS2_PLACEMENT_3D ( 'NONE', #3257, #9523, #1464 ) ;
#8190 = CARTESIAN_POINT ( 'NONE',  ( 71.82423009839129691, 30.00000000000000000, -203.8354503650404865 ) ) ;
#8191 = ORIENTED_EDGE ( 'NONE', *, *, #11372, .F. ) ;
#8192 = FACE_OUTER_BOUND ( 'NONE', #1815, .T. ) ;
#8193 = EDGE_LOOP ( 'NONE', ( #8179, #5015, #1444, #3920 ) ) ;
#8194 = CARTESIAN_POINT ( 'NONE',  ( -249.0239419981220124, 10.26696505005539350, -5.714577088569218866 ) ) ;
#8195 = CARTESIAN_POINT ( 'NONE',  ( -244.7967862068877594, -8.624712650514746670, -8.343521798357105723 ) ) ;
#8196 = PRODUCT_DEFINITION_SHAPE ( 'NONE', 'NONE',  #13092 ) ;
#8197 = AXIS2_PLACEMENT_3D ( 'NONE', #10506, #7376, #8509 ) ;
#8198 = CARTESIAN_POINT ( 'NONE',  ( -249.6369960391978680, -11.07262528782856670, 3.948341303013173764 ) ) ;
#8199 = ORIENTED_EDGE ( 'NONE', *, *, #5432, .F. ) ;
#8200 = CARTESIAN_POINT ( 'NONE',  ( -234.3927740981719978, 20.79694577626919028, 115.5625104415733944 ) ) ;
#8201 = CARTESIAN_POINT ( 'NONE',  ( -245.6532195753607084, 9.065612403116238838, -7.862145249173209116 ) ) ;
#8202 = CARTESIAN_POINT ( 'NONE',  ( -0.000000000000000000, -19.00000000000000000, 0.000000000000000000 ) ) ;
#8203 = EDGE_CURVE ( 'NONE', #6584, #10068, #3970, .T. ) ;
#8204 = CARTESIAN_POINT ( 'NONE',  ( -243.8684449830084020, -8.017731004131830375, -8.590997629223123155 ) ) ;
#8205 = EDGE_CURVE ( 'NONE', #6789, #2094, #12443, .T. ) ;
#8206 = AXIS2_PLACEMENT_3D ( 'NONE', #7280, #7476, #2341 ) ;
#8207 = DIRECTION ( 'NONE',  ( -0.000000000000000000, -1.000000000000000000, 0.000000000000000000 ) ) ;
#8208 = DIRECTION ( 'NONE',  ( -0.4226182617406911146, 0.000000000000000000, -0.9063077870366538225 ) ) ;
#8209 = CARTESIAN_POINT ( 'NONE',  ( -229.9250651581393754, -10.17993753377408872, 5.880500963262212721 ) ) ;
#8210 = EDGE_CURVE ( 'NONE', #2492, #3412, #396, .T. ) ;
#8211 = ITEM_DEFINED_TRANSFORMATION ( 'NONE', 'NONE', #647,  #805 ) ;
#8212 = CARTESIAN_POINT ( 'NONE',  ( 235.4000000000000057, -4.550331206106116078, -2.508881407069070590 ) ) ;
#8213 = ORIENTED_EDGE ( 'NONE', *, *, #2109, .F. ) ;
#8214 = EDGE_LOOP ( 'NONE', ( #6152, #5229, #2176, #11885 ) ) ;
#8215 = VECTOR ( 'NONE', #6013, 1000.000000000000000 ) ;
#8216 = CARTESIAN_POINT ( 'NONE',  ( 172.1812796676979929, 20.08915143304314910, -196.2980642831070099 ) ) ;
#8217 = CYLINDRICAL_SURFACE ( 'NONE', #4862, 5.100000000000003197 ) ;
#8218 = AXIS2_PLACEMENT_3D ( 'NONE', #6307, #2231, #9300 ) ;
#8219 = CARTESIAN_POINT ( 'NONE',  ( 31.82909658243173467, -30.00000000000000000, -285.6728570749450569 ) ) ;
#8220 = DIRECTION ( 'NONE',  ( 0.000000000000000000, 0.000000000000000000, 1.000000000000000000 ) ) ;
#8221 = CARTESIAN_POINT ( 'NONE',  ( 228.6269314446401211, -29.00000000000000000, -181.7250016321579835 ) ) ;
#8222 = CARTESIAN_POINT ( 'NONE',  ( 0.000000000000000000, 20.00000000000000000, 0.000000000000000000 ) ) ;
#8223 = DIRECTION ( 'NONE',  ( 1.000000000000000000, 0.000000000000000000, 1.047444401652940007E-14 ) ) ;
#8224 = CARTESIAN_POINT ( 'NONE',  ( -244.6749594711698705, -8.549245790843562176, 8.062606907241317344 ) ) ;
#8225 = AXIS2_PLACEMENT_3D ( 'NONE', #12847, #10523, #4445 ) ;
#8226 =( REPRESENTATION_RELATIONSHIP ('NONE','NONE', #12019, #182 ) REPRESENTATION_RELATIONSHIP_WITH_TRANSFORMATION ( #2175 )SHAPE_REPRESENTATION_RELATIONSHIP( ) );
#8227 = VERTEX_POINT ( 'NONE', #10569 ) ;
#8228 = CARTESIAN_POINT ( 'NONE',  ( 197.8197553893920144, 19.00000000000000000, 69.77553482998851564 ) ) ;
#8229 = CARTESIAN_POINT ( 'NONE',  ( -249.7118339206215012, 9.997999799959989886, -6.636264009214830395 ) ) ;
#8230 = ORIENTED_EDGE ( 'NONE', *, *, #3606, .T. ) ;
#8231 = EDGE_LOOP ( 'NONE', ( #7962, #502, #2840, #6138 ) ) ;
#8232 = CARTESIAN_POINT ( 'NONE',  ( -197.8197553893924976, 19.00000000000000000, -69.77553482998720824 ) ) ;
#8233 = CARTESIAN_POINT ( 'NONE',  ( 235.4000000000000057, 2.999417280921144346, -0.05912676983912663192 ) ) ;
#8234 = EDGE_CURVE ( 'NONE', #4193, #612, #1157, .T. ) ;
#8235 = CARTESIAN_POINT ( 'NONE',  ( 84.14846197979342435, 19.96883746137058679, -247.8175805188673735 ) ) ;
#8236 = CARTESIAN_POINT ( 'NONE',  ( -238.7978133391466429, -0.6936645309432929452, -11.97993715202083820 ) ) ;
#8237 = DIRECTION ( 'NONE',  ( -0.2588190451025213501, 0.000000000000000000, 0.9659258262890680902 ) ) ;
#8238 = CARTESIAN_POINT ( 'NONE',  ( -244.2426106971964543, 8.274791045078206508, 8.342083836226366955 ) ) ;
#8239 = EDGE_LOOP ( 'NONE', ( #2044, #2030, #10464, #8871, #6255 ) ) ;
#8240 = CARTESIAN_POINT ( 'NONE',  ( -4.572608844893758122E-13, 20.79694577634647601, 260.7745447061711275 ) ) ;
#8241 = ORIENTED_EDGE ( 'NONE', *, *, #11372, .T. ) ;
#8242 = LINE ( 'NONE', #7239, #1189 ) ;
#8243 = ORIENTED_EDGE ( 'NONE', *, *, #8350, .F. ) ;
#8244 = ORIENTED_EDGE ( 'NONE', *, *, #3436, .T. ) ;
#8245 = DIRECTION ( 'NONE',  ( 0.000000000000000000, -1.000000000000000000, 0.000000000000000000 ) ) ;
#8246 = DIRECTION ( 'NONE',  ( 1.000000000000000000, 0.000000000000000000, 0.000000000000000000 ) ) ;
#8247 = CARTESIAN_POINT ( 'NONE',  ( 239.0281511860673049, 0.5135531388252957408, 3.462181616324999212 ) ) ;
#8248 = ADVANCED_FACE ( 'NONE', ( #11642 ), #7569, .T. ) ;
#8249 = ADVANCED_FACE ( 'NONE', ( #2372 ), #1437, .T. ) ;
#8250 = FACE_OUTER_BOUND ( 'NONE', #7088, .T. ) ;
#8251 = CARTESIAN_POINT ( 'NONE',  ( -42.46883004693665953, 20.08915143297737060, -257.2112267038640425 ) ) ;
#8252 = DIRECTION ( 'NONE',  ( -0.000000000000000000, -1.000000000000000000, 0.000000000000000000 ) ) ;
#8253 = ITEM_DEFINED_TRANSFORMATION ( 'NONE', 'NONE', #8480,  #805 ) ;
#8254 = VERTEX_POINT ( 'NONE', #6445 ) ;
#8255 = LINE ( 'NONE', #6258, #1565 ) ;
#8257 = EDGE_LOOP ( 'NONE', ( #3366, #514, #1250, #8986 ) ) ;
#8256 = AXIS2_PLACEMENT_3D ( 'NONE', #12586, #12709, #524 ) ;
#8258 = CARTESIAN_POINT ( 'NONE',  ( 0.000000000000000000, 0.000000000000000000, 0.000000000000000000 ) ) ;
#8259 = DIRECTION ( 'NONE',  ( 0.000000000000000000, 0.000000000000000000, -1.000000000000000000 ) ) ;
#8260 = ADVANCED_FACE ( 'NONE', ( #2497 ), #103, .F. ) ;
#8261 = CARTESIAN_POINT ( 'NONE',  ( -249.7900429577784678, -11.65124970439946139, 1.521630468629134203 ) ) ;
#8262 = ORIENTED_EDGE ( 'NONE', *, *, #10275, .F. ) ;
#8263 = CARTESIAN_POINT ( 'NONE',  ( -34.13493237016224668, 20.79694577639865471, 259.0935598599945138 ) ) ;
#8264 = CARTESIAN_POINT ( 'NONE',  ( -242.3537289185128429, 6.680330754393353665, -9.968624625890335267 ) ) ;
#8265 = LINE ( 'NONE', #4185, #407 ) ;
#8266 = CARTESIAN_POINT ( 'NONE',  ( -242.4885533050452580, -6.811171350273821368, -9.574815118338978692 ) ) ;
#8267 = CARTESIAN_POINT ( 'NONE',  ( 239.4667603742667836, -1.483520951478357830, 3.170043417407540698 ) ) ;
#8268 = CARTESIAN_POINT ( 'NONE',  ( 34.28253040793635620, -138.4705547276867321, 24.00488622054122700 ) ) ;
#8269 = CARTESIAN_POINT ( 'NONE',  ( -229.9452934870987519, 10.90465451554996434, -5.064158863968243551 ) ) ;
#8270 = CONTEXT_DEPENDENT_SHAPE_REPRESENTATION ( #11472, #3771 ) ;
#8271 = EDGE_CURVE ( 'NONE', #2842, #7991, #5499, .T. ) ;
#8272 = AXIS2_PLACEMENT_3D ( 'NONE', #4806, #1684, #10810 ) ;
#8273 = EDGE_CURVE ( 'NONE', #9399, #3301, #2218, .T. ) ;
#8274 = FACE_OUTER_BOUND ( 'NONE', #189, .T. ) ;
#8275 = VERTEX_POINT ( 'NONE', #11380 ) ;
#8276 = ORIENTED_EDGE ( 'NONE', *, *, #5734, .T. ) ;
#8277 = CARTESIAN_POINT ( 'NONE',  ( -158.9353507248835058, 20.08915143316258778, 207.1687172305619811 ) ) ;
#8278 = CARTESIAN_POINT ( 'NONE',  ( -197.8197553893924976, 19.00000000000000000, -69.77553482998720824 ) ) ;
#8279 = CARTESIAN_POINT ( 'NONE',  ( -290.6841825403030839, -18.00000000000000000, -27.68945685411394919 ) ) ;
#8280 = DIRECTION ( 'NONE',  ( 0.000000000000000000, 0.000000000000000000, -1.000000000000000000 ) ) ;
#8281 = CONICAL_SURFACE ( 'NONE', #1456, 5.500000000000015099, 0.7853981633974461696 ) ;
#8282 = CONICAL_SURFACE ( 'NONE', #6144, 239.0000000000000000, 1.164698268477281307 ) ;
#8283 = LINE ( 'NONE', #3261, #3445 ) ;
#8284 = VECTOR ( 'NONE', #4328, 1000.000000000000000 ) ;
#8285 = AXIS2_PLACEMENT_3D ( 'NONE', #11755, #10556, #8432 ) ;
#8286 = DIRECTION ( 'NONE',  ( 0.000000000000000000, -1.000000000000000000, 0.000000000000000000 ) ) ;
#8287 = DIRECTION ( 'NONE',  ( -0.08715574274764853469, 0.000000000000000000, -0.9961946980917465444 ) ) ;
#8288 = AXIS2_PLACEMENT_3D ( 'NONE', #7882, #12081, #10884 ) ;
#8289 = DIRECTION ( 'NONE',  ( 0.000000000000000000, 1.000000000000000000, 0.000000000000000000 ) ) ;
#8290 = VERTEX_POINT ( 'NONE', #241 ) ;
#8291 = CARTESIAN_POINT ( 'NONE',  ( 240.3826708216974737, -2.772967769359219847, 2.135567781667135012 ) ) ;
#8292 = ADVANCED_FACE ( 'NONE', ( #4491 ), #7549, .F. ) ;
#8293 = CARTESIAN_POINT ( 'NONE',  ( 229.9760321542115662, -1.127100313231406803, -3.321498603606710898 ) ) ;
#8294 = ORIENTED_EDGE ( 'NONE', *, *, #7099, .T. ) ;
#8295 = ORIENTED_EDGE ( 'NONE', *, *, #5347, .T. ) ;
#8296 = AXIS2_PLACEMENT_3D ( 'NONE', #5999, #12125, #12326 ) ;
#8297 = CARTESIAN_POINT ( 'NONE',  ( 240.1760274753965518, -2.306688218040592986, 2.632364499240650968 ) ) ;
#8298 = VERTEX_POINT ( 'NONE', #2240 ) ;
#8299 = AXIS2_PLACEMENT_3D ( 'NONE', #9372, #238, #4296 ) ;
#8300 = CARTESIAN_POINT ( 'NONE',  ( 196.7513681799443361, 19.96883746182971464, 172.5787240285351345 ) ) ;
#8301 = CARTESIAN_POINT ( 'NONE',  ( 235.4000000000000057, -2.749465840844381948, 0.05419953901920007699 ) ) ;
#8302 = CARTESIAN_POINT ( 'NONE',  ( 0.000000000000000000, 0.000000000000000000, 0.000000000000000000 ) ) ;
#8303 = CARTESIAN_POINT ( 'NONE',  ( -243.2454781773737977, 7.524012760887466733, 9.025130269038724506 ) ) ;
#8304 = PRODUCT_DEFINITION_SHAPE ( 'NONE', 'NONE',  #13083 ) ;
#8305 = CONICAL_SURFACE ( 'NONE', #12974, 195.0000000000000000, 0.7853981633974476129 ) ;
#8306 = EDGE_LOOP ( 'NONE', ( #1883, #4291, #6383, #4095 ) ) ;
#8307 = CARTESIAN_POINT ( 'NONE',  ( 235.0999999999999943, 0.000000000000000000, 0.000000000000000000 ) ) ;
#8308 = VERTEX_POINT ( 'NONE', #9376 ) ;
#8309 = DIRECTION ( 'NONE',  ( 0.000000000000000000, 0.000000000000000000, -1.000000000000000000 ) ) ;
#8310 = ORIENTED_EDGE ( 'NONE', *, *, #2134, .F. ) ;
#8311 = ORIENTED_EDGE ( 'NONE', *, *, #683, .T. ) ;
#8312 = VECTOR ( 'NONE', #5130, 1000.000000000000000 ) ;
#8313 = CARTESIAN_POINT ( 'NONE',  ( -210.0000000000000000, 18.00000000000000000, 0.000000000000000000 ) ) ;
#8314 = DIRECTION ( 'NONE',  ( 0.000000000000000000, 0.000000000000000000, -1.000000000000000000 ) ) ;
#8315 = PRODUCT ( 'Slewing Ring High Pressure Lip Seals Top Bottom', 'Slewing Ring High Pressure Lip Seals Top Bottom', '', ( #8401 ) ) ;
#8316 = DIRECTION ( 'NONE',  ( -0.4503334343941556295, 0.7071067811865489050, -0.5451603414287969906 ) ) ;
#8317 = DIRECTION ( 'NONE',  ( 0.000000000000000000, 0.000000000000000000, 1.000000000000000000 ) ) ;
#8318 = DIRECTION ( 'NONE',  ( -1.000000000000000000, 0.000000000000000000, 0.000000000000000000 ) ) ;
#8319 = SURFACE_STYLE_FILL_AREA ( #4238 ) ;
#8320 = ORIENTED_EDGE ( 'NONE', *, *, #1973, .T. ) ;
#8321 = CARTESIAN_POINT ( 'NONE',  ( 235.4000000000000057, -0.05419953901919974393, -2.749465840844381948 ) ) ;
#8322 = ORIENTED_EDGE ( 'NONE', *, *, #1571, .T. ) ;
#8323 = DIRECTION ( 'NONE',  ( 8.659560562354926695E-17, -0.7071067811865480168, 0.7071067811865470176 ) ) ;
#8324 = CARTESIAN_POINT ( 'NONE',  ( -244.4094253577036113, -8.392574414408105810, -8.577616036601044769 ) ) ;
#8325 = EDGE_CURVE ( 'NONE', #4274, #823, #4299, .T. ) ;
#8326 = EDGE_CURVE ( 'NONE', #10046, #11448, #3625, .T. ) ;
#8327 = AXIS2_PLACEMENT_3D ( 'NONE', #10401, #4460, #1279 ) ;
#8328 = CARTESIAN_POINT ( 'NONE',  ( -249.7846912502906207, -11.60973349240726549, 1.810138451173344931 ) ) ;
#8329 = ORIENTED_EDGE ( 'NONE', *, *, #12032, .F. ) ;
#8330 = CARTESIAN_POINT ( 'NONE',  ( -252.4341100429120104, 20.79694577648844245, 67.61424743034129392 ) ) ;
#8331 = CARTESIAN_POINT ( 'NONE',  ( -241.4851975125052377, 5.604998872377223051, -10.61066964826765080 ) ) ;
#8332 = CYLINDRICAL_SURFACE ( 'NONE', #7633, 5.500000000000015099 ) ;
#8333 = CARTESIAN_POINT ( 'NONE',  ( -242.2164292014763305, -6.515245625945103924, -9.778246362750261156 ) ) ;
#8334 = EDGE_CURVE ( 'NONE', #7035, #3038, #12933, .T. ) ;
#8335 = CARTESIAN_POINT ( 'NONE',  ( 239.2087834361827277, -1.051957556907570090, 3.338183402683874146 ) ) ;
#8336 = DIRECTION ( 'NONE',  ( 0.2154914511802761279, 0.5538822189107472926, 0.8042250444015818234 ) ) ;
#8337 = DIRECTION ( 'NONE',  ( -1.000000000000000000, -0.000000000000000000, -0.000000000000000000 ) ) ;
#8338 = AXIS2_PLACEMENT_3D ( 'NONE', #2826, #2692, #9969 ) ;
#8339 = DIRECTION ( 'NONE',  ( 0.000000000000000000, 0.9998057603070481525, -0.01970892327970899874 ) ) ;
#8340 = ORIENTED_EDGE ( 'NONE', *, *, #5260, .F. ) ;
#8341 = CONICAL_SURFACE ( 'NONE', #247, 6.500000000000005329, 0.7853981633974490562 ) ;
#8342 = ORIENTED_EDGE ( 'NONE', *, *, #2924, .F. ) ;
#8343 = CARTESIAN_POINT ( 'NONE',  ( -84.14846197923118609, 19.96883746246331981, 247.8175805181506348 ) ) ;
#8344 = CARTESIAN_POINT ( 'NONE',  ( 225.1241593668336236, -19.00000000000000000, -185.9653539489990521 ) ) ;
#8345 = CARTESIAN_POINT ( 'NONE',  ( 3.053044470274351535E-14, 30.00000000000000000, 248.7999999999999829 ) ) ;
#8346 = CARTESIAN_POINT ( 'NONE',  ( 239.2711857403947988, -1.179132569181245316, -3.296284915250143221 ) ) ;
#8347 = CARTESIAN_POINT ( 'NONE',  ( 71.82423009839129691, 19.40000000000000213, -197.3354503650404865 ) ) ;
#8348 = ADVANCED_FACE ( 'NONE', ( #11895 ), #2009, .F. ) ;
#8349 = DIRECTION ( 'NONE',  ( 0.000000000000000000, 0.000000000000000000, -1.000000000000000000 ) ) ;
#8350 = EDGE_CURVE ( 'NONE', #12027, #2438, #3707, .T. ) ;
#8351 = CARTESIAN_POINT ( 'NONE',  ( -197.8197553893909912, 30.00000000000000000, 64.27553482999130097 ) ) ;
#8352 = DIRECTION ( 'NONE',  ( 0.1736481776669172861, 0.000000000000000000, 0.9848077530122105738 ) ) ;
#8353 = DIRECTION ( 'NONE',  ( 0.000000000000000000, 1.000000000000000000, 0.000000000000000000 ) ) ;
#8354 = ITEM_DEFINED_TRANSFORMATION ( 'NONE', 'NONE', #12953,  #805 ) ;
#8355 = B_SPLINE_CURVE_WITH_KNOTS ( 'NONE', 3,
 ( #10972, #7897, #3901, #2958, #11970, #6043, #3762, #12037, #840, #2144, #2750, #2889, #10096, #1842, #6839, #8839, #11031, #10900, #970, #12167, #5846, #778, #11099 ),
 .UNSPECIFIED., .F., .F.,
 ( 4, 2, 2, 1, 1, 2, 2, 2, 2, 1, 2, 2, 4 ),
 ( 0.000000000000000000, 0.06250953674349737921, 0.09376430511523958788, 0.1093916893011107061, 0.1172053813940463346, 0.1211122274405143084, 0.1250190734869822962, 0.1875286102303734270, 0.2187833786020739191, 0.2344107627879288558, 0.2422244548808562548, 0.2500381469737836260, 0.5000762939474624469 ),
 .UNSPECIFIED. ) ;
#8356 = EDGE_LOOP ( 'NONE', ( #7005, #12544, #1053 ) ) ;
#8357 = LINE ( 'NONE', #7284, #1715 ) ;
#8358 = CARTESIAN_POINT ( 'NONE',  ( 229.9733680233430846, -0.2312567328850919368, 3.499999999999965361 ) ) ;
#8359 = ORIENTED_EDGE ( 'NONE', *, *, #8511, .T. ) ;
#8360 = VERTEX_POINT ( 'NONE', #4818 ) ;
#8361 = DIRECTION ( 'NONE',  ( 0.000000000000000000, 0.000000000000000000, 1.000000000000000000 ) ) ;
#8362 = LINE ( 'NONE', #6554, #6544 ) ;
#8363 = CARTESIAN_POINT ( 'NONE',  ( 67.71318189785222330, 19.96883746181513786, 252.8031682274115042 ) ) ;
#8364 = ADVANCED_FACE ( 'NONE', ( #6642 ), #7631, .F. ) ;
#8365 = DIRECTION ( 'NONE',  ( 0.000000000000000000, -1.000000000000000000, 0.000000000000000000 ) ) ;
#8366 = DIRECTION ( 'NONE',  ( 0.9396926207859080948, 0.000000000000000000, 0.3420201433256694346 ) ) ;
#8367 = CIRCLE ( 'NONE', #10903, 250.1999999999999602 ) ;
#8368 = B_SPLINE_CURVE_WITH_KNOTS ( 'NONE', 3,
 ( #8013, #2620, #3691, #9620, #9687, #8078, #703, #6707 ),
 .UNSPECIFIED., .F., .F.,
 ( 4, 2, 2, 4 ),
 ( 0.000000000000000000, 0.2500000000000095479, 0.5000000000000190958, 1.000000000000000000 ),
 .UNSPECIFIED. ) ;
#8369 = CARTESIAN_POINT ( 'NONE',  ( 122.2593324768334071, 30.00000000000000000, -168.2755348299895104 ) ) ;
#8370 = ORIENTED_EDGE ( 'NONE', *, *, #2370, .T. ) ;
#8371 = CARTESIAN_POINT ( 'NONE',  ( 221.5672498511021047, 20.79694577634646890, 137.7829567244531574 ) ) ;
#8372 = EDGE_CURVE ( 'NONE', #2275, #6648, #12862, .T. ) ;
#8373 = ORIENTED_EDGE ( 'NONE', *, *, #8746, .T. ) ;
#8374 = DIRECTION ( 'NONE',  ( 0.6368676505102716101, 0.000000000000000000, 0.7709731485165527420 ) ) ;
#8375 = ORIENTED_EDGE ( 'NONE', *, *, #5385, .F. ) ;
#8376 = ORIENTED_EDGE ( 'NONE', *, *, #12569, .F. ) ;
#8377 = AXIS2_PLACEMENT_3D ( 'NONE', #7947, #13011, #10011 ) ;
#8378 = MECHANICAL_DESIGN_GEOMETRIC_PRESENTATION_REPRESENTATION (  '', ( #713 ), #7725 ) ;
#8379 = DIRECTION ( 'NONE',  ( 1.000000000000000000, 0.000000000000000000, 0.000000000000000000 ) ) ;
#8380 = FACE_BOUND ( 'NONE', #8386, .T. ) ;
#8381 = DIRECTION ( 'NONE',  ( 0.6368676505102716101, 0.000000000000000000, 0.7709731485165527420 ) ) ;
#8382 = LINE ( 'NONE', #11438, #6662 ) ;
#8383 = CARTESIAN_POINT ( 'NONE',  ( -238.7112176159036778, 0.03609691783649805058, -11.74994919738963439 ) ) ;
#8384 = CARTESIAN_POINT ( 'NONE',  ( -242.9129853713322973, 7.240649582117769434, 9.569633193565069362 ) ) ;
#8385 = AXIS2_PLACEMENT_3D ( 'NONE', #10572, #641, #4693 ) ;
#8386 = EDGE_LOOP ( 'NONE', ( #1002, #8903 ) ) ;
#8387 = AXIS2_PLACEMENT_3D ( 'NONE', #10533, #12467, #11672 ) ;
#8388 = CARTESIAN_POINT ( 'NONE',  ( 6.735557395310435121E-16, 19.00000000000000000, 202.4999999999999716 ) ) ;
#8389 = ORIENTED_EDGE ( 'NONE', *, *, #2540, .T. ) ;
#8390 = DIRECTION ( 'NONE',  ( 0.000000000000000000, 0.000000000000000000, 1.000000000000000000 ) ) ;
#8391 = CARTESIAN_POINT ( 'NONE',  ( -194.2446334056326123, -19.00000000000000000, -235.1468102975487682 ) ) ;
#8392 = CARTESIAN_POINT ( 'NONE',  ( 253.8843055347119275, 20.08915143297736705, -59.19439222780434307 ) ) ;
#8393 = ORIENTED_EDGE ( 'NONE', *, *, #140, .F. ) ;
#8394 = VECTOR ( 'NONE', #6170, 1000.000000000000000 ) ;
#8395 = CARTESIAN_POINT ( 'NONE',  ( 0.000000000000000000, 0.000000000000000000, 0.000000000000000000 ) ) ;
#8396 = CARTESIAN_POINT ( 'NONE',  ( 197.8197553893915028, 29.00000000000000000, -69.77553482998990830 ) ) ;
#8397 = CARTESIAN_POINT ( 'NONE',  ( 5.000000000000000000, 0.000000000000000000, 250.0000000000000000 ) ) ;
#8398 = CARTESIAN_POINT ( 'NONE',  ( -229.9801196668058481, 11.35475723081091992, 3.046485053526966968 ) ) ;
#8399 = EDGE_CURVE ( 'NONE', #11942, #12887, #9826, .T. ) ;
#8400 = DIRECTION ( 'NONE',  ( 0.6368676505102707219, 0.000000000000000000, 0.7709731485165535192 ) ) ;
#8401 = PRODUCT_CONTEXT ( 'NONE', #8164, 'mechanical' ) ;
#8402 = CARTESIAN_POINT ( 'NONE',  ( -229.6930204784227385, 1.737490451635691713, -11.87941726754192828 ) ) ;
#8403 = AXIS2_PLACEMENT_3D ( 'NONE', #5305, #9560, #443 ) ;
#8404 = DIRECTION ( 'NONE',  ( 0.000000000000000000, 1.000000000000000000, 0.000000000000000000 ) ) ;
#8405 = ORIENTED_EDGE ( 'NONE', *, *, #7066, .F. ) ;
#8406 = CARTESIAN_POINT ( 'NONE',  ( 252.2208631679619941, 20.08915143265656766, 67.55708173926319660 ) ) ;
#8407 = CARTESIAN_POINT ( 'NONE',  ( 212.6409525001303962, -25.00000000000000000, 138.9238112054132159 ) ) ;
#8408 = FACE_OUTER_BOUND ( 'NONE', #4402, .T. ) ;
#8409 = CARTESIAN_POINT ( 'NONE',  ( -249.2689385757807941, 10.50219330951863306, 5.269387968809968292 ) ) ;
#8410 = DIRECTION ( 'NONE',  ( 0.000000000000000000, -1.000000000000000000, 0.000000000000000000 ) ) ;
#8411 = CIRCLE ( 'NONE', #11167, 6.500000000000005329 ) ;
#8412 = DIRECTION ( 'NONE',  ( 1.000000000000000000, 0.000000000000000000, 0.000000000000000000 ) ) ;
#8413 = CARTESIAN_POINT ( 'NONE',  ( -246.4205552533093169, -9.380328321255895219, 7.484021895908157695 ) ) ;
#8414 = ADVANCED_FACE ( 'NONE', ( #5768 ), #2839, .T. ) ;
#8415 = DIRECTION ( 'NONE',  ( 0.6368676505102695007, 0.000000000000000000, 0.7709731485165545184 ) ) ;
#8416 = CARTESIAN_POINT ( 'NONE',  ( -34.28253040793669015, -138.4705547276867321, 24.00488622054075805 ) ) ;
#8417 = CARTESIAN_POINT ( 'NONE',  ( 197.8197553893915028, 29.00000000000000000, -58.77553482998990830 ) ) ;
#8418 = ITEM_DEFINED_TRANSFORMATION ( 'NONE', 'NONE', #4864,  #805 ) ;
#8419 = ORIENTED_EDGE ( 'NONE', *, *, #9595, .T. ) ;
#8420 = CARTESIAN_POINT ( 'NONE',  ( 0.000000000000000000, 18.00000000000000000, 201.4999999999999716 ) ) ;
#8421 = PRODUCT_DEFINITION_SHAPE ( 'NONE', 'NONE',  #13068 ) ;
#8422 = CARTESIAN_POINT ( 'NONE',  ( 229.9901773315476987, -2.783473308305698168, -2.134081248093457006 ) ) ;
#8423 = ORIENTED_EDGE ( 'NONE', *, *, #1510, .F. ) ;
#8424 = VERTEX_POINT ( 'NONE', #2561 ) ;
#8425 = EDGE_CURVE ( 'NONE', #3933, #4419, #2815, .T. ) ;
#8426 = DIRECTION ( 'NONE',  ( -0.000000000000000000, -1.000000000000000000, 0.000000000000000000 ) ) ;
#8427 = PLANE ( 'NONE',  #9972 ) ;
#8428 = UNCERTAINTY_MEASURE_WITH_UNIT (LENGTH_MEASURE( 1.000000000000000082E-05 ), #707, 'distance_accuracy_value', 'NONE');
#8429 = CARTESIAN_POINT ( 'NONE',  ( -234.8993005728878529, 20.55460285095910677, 115.8123742916932741 ) ) ;
#8430 = AXIS2_PLACEMENT_3D ( 'NONE', #8783, #6661, #10719 ) ;
#8431 = DIRECTION ( 'NONE',  ( 0.6368676505102695007, 0.000000000000000000, 0.7709731485165545184 ) ) ;
#8432 = DIRECTION ( 'NONE',  ( -0.1736481776669340227, 0.000000000000000000, 0.9848077530122074652 ) ) ;
#8433 = CIRCLE ( 'NONE', #2660, 254.1999999999999886 ) ;
#8434 = CARTESIAN_POINT ( 'NONE',  ( -197.8197553893924976, 30.00000000000000000, -69.77553482998720824 ) ) ;
#8435 = CARTESIAN_POINT ( 'NONE',  ( -244.1900186690936323, 20.79694577634646180, 91.90986972409903899 ) ) ;
#8436 = ORIENTED_EDGE ( 'NONE', *, *, #3506, .T. ) ;
#8437 = ORIENTED_EDGE ( 'NONE', *, *, #9245, .F. ) ;
#8438 = DIRECTION ( 'NONE',  ( -0.000000000000000000, -1.000000000000000000, 0.000000000000000000 ) ) ;
#8439 = ORIENTED_EDGE ( 'NONE', *, *, #9485, .T. ) ;
#8440 = EDGE_LOOP ( 'NONE', ( #10206, #255, #6892, #7269 ) ) ;
#8441 = EDGE_CURVE ( 'NONE', #3706, #10670, #1700, .T. ) ;
#8442 = EDGE_CURVE ( 'NONE', #12258, #5446, #12895, .T. ) ;
#8443 = SHAPE_REPRESENTATION ( 'Slewing Ring High Pressure Lip Seals Top', ( #805 ), #391 ) ;
#8444 = DIRECTION ( 'NONE',  ( 0.000000000000000000, -1.000000000000000000, 0.000000000000000000 ) ) ;
#8445 = CARTESIAN_POINT ( 'NONE',  ( 229.9000000000000057, -0.6143654365053307087, -4.885954882152276468 ) ) ;
#8446 = DIRECTION ( 'NONE',  ( 0.000000000000000000, -0.4828344519120574274, 0.8757116489157735773 ) ) ;
#8447 = CARTESIAN_POINT ( 'NONE',  ( 238.9937480947141353, 0.3586231075815122793, -3.486222115670320587 ) ) ;
#8448 = ADVANCED_FACE ( 'NONE', ( #10966 ), #5697, .F. ) ;
#8449 = DIRECTION ( 'NONE',  ( 0.000000000000000000, 0.000000000000000000, -1.000000000000000000 ) ) ;
#8450 = CARTESIAN_POINT ( 'NONE',  ( -247.8064210922640882, 9.777989738606054360, 6.956369377637167339 ) ) ;
#8451 = CARTESIAN_POINT ( 'NONE',  ( 0.000000000000000000, 11.79660968244690089, 0.000000000000000000 ) ) ;
#8452 = ITEM_DEFINED_TRANSFORMATION ( 'NONE', 'NONE', #6358,  #805 ) ;
#8453 = ORIENTED_EDGE ( 'NONE', *, *, #5225, .T. ) ;
#8454 = DIRECTION ( 'NONE',  ( 0.000000000000000000, 0.000000000000000000, -1.000000000000000000 ) ) ;
#8455 = VERTEX_POINT ( 'NONE', #7820 ) ;
#8456 = PRODUCT_DEFINITION_SHAPE ( 'NONE', 'NONE',  #13179 ) ;
#8457 = DIRECTION ( 'NONE',  ( 0.5469441386039890496, 0.000000000000000000, -0.8371691043312220470 ) ) ;
#8458 = CARTESIAN_POINT ( 'NONE',  ( 0.000000000000000000, 1.848645179567965036, 239.8169934640517624 ) ) ;
#8459 = EDGE_CURVE ( 'NONE', #2079, #11730, #706, .T. ) ;
#8460 = CARTESIAN_POINT ( 'NONE',  ( 243.9837273761028769, 20.08915143297736705, 91.83222442980245148 ) ) ;
#8461 = ORIENTED_EDGE ( 'NONE', *, *, #4031, .T. ) ;
#8462 = FACE_OUTER_BOUND ( 'NONE', #11831, .T. ) ;
#8463 = CARTESIAN_POINT ( 'NONE',  ( -241.3346421314153076, 5.383590977540964495, -10.72461093951445399 ) ) ;
#8464 = CARTESIAN_POINT ( 'NONE',  ( -239.0315606904630954, 1.240325117213125328, 11.93572853651427756 ) ) ;
#8465 = DIRECTION ( 'NONE',  ( 0.000000000000000000, 1.000000000000000000, 0.000000000000000000 ) ) ;
#8466 = APPLICATION_PROTOCOL_DEFINITION ( 'draft international standard', 'automotive_design', 1998, #2943 ) ;
#8467 = CARTESIAN_POINT ( 'NONE',  ( 240.3826708216974737, 2.772967769358989809, -2.135567781667440102 ) ) ;
#8468 = FACE_OUTER_BOUND ( 'NONE', #1288, .T. ) ;
#8469 = VERTEX_POINT ( 'NONE', #4689 ) ;
#8470 = AXIS2_PLACEMENT_3D ( 'NONE', #2636, #8713, #6977 ) ;
#8471 = CARTESIAN_POINT ( 'NONE',  ( 159.3024069666089133, 19.96883745889249795, 207.6469600140662806 ) ) ;
#8472 = CARTESIAN_POINT ( 'NONE',  ( 0.000000000000000000, 22.00000000000000000, 0.000000000000000000 ) ) ;
#8473 = DIRECTION ( 'NONE',  ( -0.7709731485165534082, 0.000000000000000000, 0.6368676505102708330 ) ) ;
#8474 =( REPRESENTATION_RELATIONSHIP ('NONE','NONE', #12019, #182 ) REPRESENTATION_RELATIONSHIP_WITH_TRANSFORMATION ( #1184 )SHAPE_REPRESENTATION_RELATIONSHIP( ) );
#8475 = CARTESIAN_POINT ( 'NONE',  ( 3.059167704270088292E-14, 21.50000000000000000, 249.7999999999999829 ) ) ;
#8476 = CARTESIAN_POINT ( 'NONE',  ( 294.8238222686200061, -30.00000000000000000, 32.70078231946946090 ) ) ;
#8477 = DIRECTION ( 'NONE',  ( 1.000000000000000000, 0.000000000000000000, 0.000000000000000000 ) ) ;
#8478 = DIRECTION ( 'NONE',  ( 0.4226182617406972208, 0.000000000000000000, 0.9063077870366510469 ) ) ;
#8479 = FACE_OUTER_BOUND ( 'NONE', #8808, .T. ) ;
#8480 = AXIS2_PLACEMENT_3D ( 'NONE', #12487, #6431, #2546 ) ;
#8481 = DIRECTION ( 'NONE',  ( 0.000000000000000000, 1.000000000000000000, 0.000000000000000000 ) ) ;
#8482 = FACE_OUTER_BOUND ( 'NONE', #11501, .T. ) ;
#8483 = ORIENTED_EDGE ( 'NONE', *, *, #11661, .F. ) ;
#8484 = ADVANCED_FACE ( 'NONE', ( #12696 ), #3926, .F. ) ;
#8485 = EDGE_LOOP ( 'NONE', ( #3472, #10899 ) ) ;
#8486 = ADVANCED_FACE ( 'NONE', ( #570 ), #10698, .T. ) ;
#8487 = CARTESIAN_POINT ( 'NONE',  ( 0.000000000000000000, 11.79660968244693997, 0.000000000000000000 ) ) ;
#8488 = FACE_BOUND ( 'NONE', #5036, .T. ) ;
#8489 = VECTOR ( 'NONE', #11750, 1000.000000000000000 ) ;
#8490 = AXIS2_PLACEMENT_3D ( 'NONE', #8344, #12466, #206 ) ;
#8491 = AXIS2_PLACEMENT_3D ( 'NONE', #6498, #12552, #5484 ) ;
#8492 = CARTESIAN_POINT ( 'NONE',  ( -207.7919029851962023, 20.55460285100346596, -159.4136521840017906 ) ) ;
#8493 = CARTESIAN_POINT ( 'NONE',  ( 0.000000000000000000, 11.79660968244690089, 0.000000000000000000 ) ) ;
#8494 = DIRECTION ( 'NONE',  ( 0.3420201433256663259, 0.000000000000000000, 0.9396926207859093161 ) ) ;
#8495 = CARTESIAN_POINT ( 'NONE',  ( 132.6365829178909621, -19.40000000000000213, -260.1259780660157048 ) ) ;
#8496 = CARTESIAN_POINT ( 'NONE',  ( -225.9597979674045973, 20.79694577634646535, 130.4544329367265334 ) ) ;
#8497 = VERTEX_POINT ( 'NONE', #12762 ) ;
#8498 = FACE_OUTER_BOUND ( 'NONE', #4027, .T. ) ;
#8500 = ORIENTED_EDGE ( 'NONE', *, *, #5328, .T. ) ;
#8499 = CIRCLE ( 'NONE', #5942, 3.000000000000000000 ) ;
#8501 = DIRECTION ( 'NONE',  ( 0.4503334343941595153, -0.7071067811865431318, 0.5451603414288016536 ) ) ;
#8502 = EDGE_LOOP ( 'NONE', ( #12816, #10816, #5152, #11954 ) ) ;
#8503 = ORIENTED_EDGE ( 'NONE', *, *, #10701, .F. ) ;
#8504 = CIRCLE ( 'NONE', #10189, 259.6078431372549744 ) ;
#8505 = VECTOR ( 'NONE', #8598, 1000.000000000000000 ) ;
#8506 = CARTESIAN_POINT ( 'NONE',  ( 135.8846079354933352, -30.00000000000000000, -256.1940150085812888 ) ) ;
#8507 = LINE ( 'NONE', #239, #6815 ) ;
#8508 = CARTESIAN_POINT ( 'NONE',  ( -286.5648042451072115, -28.60000000000000142, 14.34944810630077505 ) ) ;
#8509 = DIRECTION ( 'NONE',  ( 0.000000000000000000, -0.9998057603070480415, 0.01970892327970911323 ) ) ;
#8510 = CARTESIAN_POINT ( 'NONE',  ( 294.1869546181097235, -29.00000000000000000, 31.92980917095288618 ) ) ;
#8511 = EDGE_CURVE ( 'NONE', #157, #1185, #2744, .T. ) ;
#8512 = ADVANCED_FACE ( 'NONE', ( #1770 ), #2850, .F. ) ;
#8513 = AXIS2_PLACEMENT_3D ( 'NONE', #3203, #1216, #11349 ) ;
#8514 = ITEM_DEFINED_TRANSFORMATION ( 'NONE', 'NONE', #5503,  #805 ) ;
#8515 = VERTEX_POINT ( 'NONE', #100 ) ;
#8516 = DIRECTION ( 'NONE',  ( -0.000000000000000000, -1.000000000000000000, 0.000000000000000000 ) ) ;
#8517 = ORIENTED_EDGE ( 'NONE', *, *, #5236, .T. ) ;
#8518 = LINE ( 'NONE', #5174, #4009 ) ;
#8519 = FACE_OUTER_BOUND ( 'NONE', #1613, .T. ) ;
#8520 = AXIS2_PLACEMENT_3D ( 'NONE', #12341, #9138, #15 ) ;
#8521 = CARTESIAN_POINT ( 'NONE',  ( 243.9837273761030474, 20.08915143297736705, -91.83222442980216726 ) ) ;
#8522 = CIRCLE ( 'NONE', #2746, 248.1666666666679930 ) ;
#8523 = DIRECTION ( 'NONE',  ( -1.000000000000000000, 0.000000000000000000, 0.000000000000000000 ) ) ;
#8524 = CARTESIAN_POINT ( 'NONE',  ( -241.3656950238681134, 5.430352949065432533, -10.70105707677310924 ) ) ;
#8525 = CARTESIAN_POINT ( 'NONE',  ( -193.6077657551222728, -30.00000000000000000, -234.3758371490322645 ) ) ;
#8526 = DIRECTION ( 'NONE',  ( 0.6368676505102707219, 0.000000000000000000, 0.7709731485165535192 ) ) ;
#8527 = ADVANCED_FACE ( 'NONE', ( #9032 ), #6231, .F. ) ;
#8528 = CARTESIAN_POINT ( 'NONE',  ( 197.8197553893915028, 19.00000000000000000, -69.77553482998990830 ) ) ;
#8529 = PRODUCT_DEFINITION_SHAPE ( 'NONE', 'NONE',  #2767 ) ;
#8530 = CARTESIAN_POINT ( 'NONE',  ( -229.7803353249896361, 6.565431021940706380, -10.05160335400266369 ) ) ;
#8531 = CONTEXT_DEPENDENT_SHAPE_REPRESENTATION ( #9956, #8456 ) ;
#8532 = AXIS2_PLACEMENT_3D ( 'NONE', #10861, #12927, #8938 ) ;
#8533 = EDGE_CURVE ( 'NONE', #9382, #10885, #5148, .T. ) ;
#8534 = CIRCLE ( 'NONE', #1291, 239.8169934640564804 ) ;
#8535 = DIRECTION ( 'NONE',  ( 0.000000000000000000, 0.000000000000000000, 1.000000000000000000 ) ) ;
#8536 = ORIENTED_EDGE ( 'NONE', *, *, #12084, .T. ) ;
#8537 = CARTESIAN_POINT ( 'NONE',  ( 226.6392846532197325, 19.96883746219288724, -130.8783844621844707 ) ) ;
#8538 = CARTESIAN_POINT ( 'NONE',  ( -31.82909658242962792, -30.00000000000000000, 285.6728570749452274 ) ) ;
#8539 = DIRECTION ( 'NONE',  ( -0.000000000000000000, -1.000000000000000000, 0.000000000000000000 ) ) ;
#8540 = DIRECTION ( 'NONE',  ( 0.000000000000000000, 0.9998057603070480415, -0.01970892327970899874 ) ) ;
#8541 = ORIENTED_EDGE ( 'NONE', *, *, #5806, .T. ) ;
#8542 = CARTESIAN_POINT ( 'NONE',  ( -260.5542428351132003, 20.08915143297736705, 8.526617657837524789 ) ) ;
#8543 = CARTESIAN_POINT ( 'NONE',  ( -159.3442861576697283, 0.000000000000000000, -192.8974817588416499 ) ) ;
#8544 = DIRECTION ( 'NONE',  ( -0.8294267566935208391, 0.5538822189107471816, -0.07256543843576089559 ) ) ;
#8545 = CARTESIAN_POINT ( 'NONE',  ( -238.7109915808064500, 2.244475480116206709E-14, 11.74999999995203126 ) ) ;
#8546 = DIRECTION ( 'NONE',  ( 0.000000000000000000, 0.000000000000000000, 1.000000000000000000 ) ) ;
#8547 = CONICAL_SURFACE ( 'NONE', #1948, 6.500000000000026645, 0.7853981633974476129 ) ;
#8548 = CARTESIAN_POINT ( 'NONE',  ( -239.0407087255592842, -1.256038987220895020, 11.93408471358068113 ) ) ;
#8549 = CARTESIAN_POINT ( 'NONE',  ( 235.4000000000000057, 2.749465840844381948, -0.05419953901919974393 ) ) ;
#8550 = VERTEX_POINT ( 'NONE', #33 ) ;
#8551 = ORIENTED_EDGE ( 'NONE', *, *, #2059, .F. ) ;
#8552 = FACE_OUTER_BOUND ( 'NONE', #6199, .T. ) ;
#8553 = FACE_OUTER_BOUND ( 'NONE', #5723, .T. ) ;
#8554 = AXIS2_PLACEMENT_3D ( 'NONE', #9169, #47, #12170 ) ;
#8555 = CARTESIAN_POINT ( 'NONE',  ( -261.3381329044966606, 20.55460285116648933, 17.10461161605900671 ) ) ;
#8556 = AXIS2_PLACEMENT_3D ( 'NONE', #10230, #10931, #2986 ) ;
#8557 = CARTESIAN_POINT ( 'NONE',  ( 227.3999999999999773, 0.1024105694487990187, 5.195143123655512341 ) ) ;
#8558 = PRODUCT_DEFINITION_SHAPE ( 'NONE', 'NONE',  #13186 ) ;
#8559 = DIRECTION ( 'NONE',  ( -0.8660254037844415942, 0.000000000000000000, 0.4999999999999949485 ) ) ;
#8560 = DIRECTION ( 'NONE',  ( 1.000000000000000000, 0.000000000000000000, 0.000000000000000000 ) ) ;
#8561 = CONICAL_SURFACE ( 'NONE', #5367, 3.823498366181860231, 0.7853981633974476129 ) ;
#8562 = CARTESIAN_POINT ( 'NONE',  ( -42.50473797389807373, 20.79694577634647246, 257.4287020129720531 ) ) ;
#8563 = ADVANCED_FACE ( 'NONE', ( #3013 ), #5582, .F. ) ;
#8564 = ORIENTED_EDGE ( 'NONE', *, *, #4821, .F. ) ;
#8565 = CARTESIAN_POINT ( 'NONE',  ( 83.86521783953205045, 20.79694577634646180, -247.0684411393754942 ) ) ;
#8566 = EDGE_LOOP ( 'NONE', ( #11429, #4164, #5895, #11645 ) ) ;
#8567 = CARTESIAN_POINT ( 'NONE',  ( -287.1814104624966149, -29.00000000000000000, -23.44910453727292321 ) ) ;
#8568 = EDGE_LOOP ( 'NONE', ( #3207, #449, #1312, #9233 ) ) ;
#8569 = ORIENTED_EDGE ( 'NONE', *, *, #11735, .F. ) ;
#8570 = CIRCLE ( 'NONE', #481, 250.1999999999999602 ) ;
#8571 = LINE ( 'NONE', #10361, #1739 ) ;
#8572 = PLANE ( 'NONE',  #3815 ) ;
#8573 = CIRCLE ( 'NONE', #4308, 249.7999999999999829 ) ;
#8574 = CARTESIAN_POINT ( 'NONE',  ( 239.7985776503625175, 1.848645179571945185, -2.971954070985139751 ) ) ;
#8575 = CARTESIAN_POINT ( 'NONE',  ( 0.000000000000000000, 0.000000000000000000, 0.000000000000000000 ) ) ;
#8576 = LINE ( 'NONE', #12637, #9848 ) ;
#8577 = EDGE_CURVE ( 'NONE', #6957, #7354, #10911, .T. ) ;
#8578 = CONTEXT_DEPENDENT_SHAPE_REPRESENTATION ( #8474, #7848 ) ;
#8579 = ORIENTED_EDGE ( 'NONE', *, *, #1085, .F. ) ;
#8580 = DIRECTION ( 'NONE',  ( 1.000000000000000000, 0.000000000000000000, 0.000000000000000000 ) ) ;
#8581 = AXIS2_PLACEMENT_3D ( 'NONE', #4805, #12940, #6756 ) ;
#8582 =( REPRESENTATION_RELATIONSHIP ('NONE','NONE', #12019, #5191 ) REPRESENTATION_RELATIONSHIP_WITH_TRANSFORMATION ( #6942 )SHAPE_REPRESENTATION_RELATIONSHIP( ) );
#8583 = EDGE_LOOP ( 'NONE', ( #4219, #9179, #7483, #959 ) ) ;
#8584 = PRESENTATION_LAYER_ASSIGNMENT (  '', '', ( #713 ) ) ;
#8585 = DIRECTION ( 'NONE',  ( 0.000000000000000000, -1.000000000000000000, 0.000000000000000000 ) ) ;
#8586 = LINE ( 'NONE', #12644, #2338 ) ;
#8587 = EDGE_CURVE ( 'NONE', #7035, #9508, #4098, .T. ) ;
#8588 = EDGE_CURVE ( 'NONE', #12985, #6295, #12205, .T. ) ;
#8589 = DIRECTION ( 'NONE',  ( 0.6368676505102708330, 0.000000000000000000, 0.7709731485165535192 ) ) ;
#8590 = CARTESIAN_POINT ( 'NONE',  ( -238.9851262181995821, 1.156799816864296115, 11.94414832311762709 ) ) ;
#8591 = AXIS2_PLACEMENT_3D ( 'NONE', #5066, #1879, #9209 ) ;
#8592 = CARTESIAN_POINT ( 'NONE',  ( -240.4375400851813822, -3.701007121282966494, -11.16264886370965570 ) ) ;
#8593 = TOROIDAL_SURFACE ( 'NONE', #9858, 250.0000000000000000, 10.00000000000000000 ) ;
#8594 = LINE ( 'NONE', #10649, #3300 ) ;
#8595 = DIRECTION ( 'NONE',  ( 0.2847642722309760566, 0.5538822189107471816, 0.7823834078220662791 ) ) ;
#8596 = CARTESIAN_POINT ( 'NONE',  ( -229.9963607380661870, 11.93083377190782279, 1.487518229564186445 ) ) ;
#8597 = AXIS2_PLACEMENT_3D ( 'NONE', #6368, #10424, #7237 ) ;
#8598 = DIRECTION ( 'NONE',  ( 8.659560562354926695E-17, 0.7071067811865480168, -0.7071067811865470176 ) ) ;
#8599 = EDGE_LOOP ( 'NONE', ( #12356, #7654 ) ) ;
#8600 = EDGE_CURVE ( 'NONE', #10757, #2690, #8966, .T. ) ;
#8601 = CARTESIAN_POINT ( 'NONE',  ( 261.1558126970361400, 19.96883746059272724, 17.09264059808175062 ) ) ;
#8602 = EDGE_CURVE ( 'NONE', #11730, #2539, #8570, .T. ) ;
#8603 = CARTESIAN_POINT ( 'NONE',  ( 197.8197553893915028, 29.00000000000000000, -64.27553482998990830 ) ) ;
#8604 = CARTESIAN_POINT ( 'NONE',  ( -197.8197553893924976, 19.00000000000000000, -64.27553482998719403 ) ) ;
#8605 =( REPRESENTATION_RELATIONSHIP ('NONE','NONE', #12019, #5191 ) REPRESENTATION_RELATIONSHIP_WITH_TRANSFORMATION ( #4842 )SHAPE_REPRESENTATION_RELATIONSHIP( ) );
#8606 = CARTESIAN_POINT ( 'NONE',  ( -225.1241593668336236, -29.00000000000000000, 185.9653539489990521 ) ) ;
#8607 = CARTESIAN_POINT ( 'NONE',  ( -42.46883004693748376, 20.08915143297736705, 257.2112267038638720 ) ) ;
#8608 = AXIS2_PLACEMENT_3D ( 'NONE', #4973, #10043, #6110 ) ;
#8609 = EDGE_CURVE ( 'NONE', #2972, #564, #6874, .T. ) ;
#8610 = DIRECTION ( 'NONE',  ( -0.000000000000000000, -1.000000000000000000, 0.000000000000000000 ) ) ;
#8611 = DIRECTION ( 'NONE',  ( 0.9396926207859080948, 0.000000000000000000, 0.3420201433256694346 ) ) ;
#8612 = CARTESIAN_POINT ( 'NONE',  ( -229.7367722661449250, -4.144097499581555155, -11.00169393300851084 ) ) ;
#8613 = CIRCLE ( 'NONE', #1801, 5.100000000000017408 ) ;
#8614 = CARTESIAN_POINT ( 'NONE',  ( -31.82909658242962081, -18.00000000000000000, 285.6728570749452274 ) ) ;
#8615 = CARTESIAN_POINT ( 'NONE',  ( 71.82423009839129691, 18.00000000000000000, 197.3354503650404865 ) ) ;
#8616 = ORIENTED_EDGE ( 'NONE', *, *, #4064, .F. ) ;
#8617 = ORIENTED_EDGE ( 'NONE', *, *, #13037, .F. ) ;
#8618 = CONICAL_SURFACE ( 'NONE', #7085, 6.500000000000005329, 0.7853981633974547183 ) ;
#8619 = AXIS2_PLACEMENT_3D ( 'NONE', #11614, #12604, #3464 ) ;
#8620 = CARTESIAN_POINT ( 'NONE',  ( -225.1241593668336236, -30.00000000000000000, 185.9653539489990521 ) ) ;
#8621 = CARTESIAN_POINT ( 'NONE',  ( 0.000000000000000000, 29.00000000000000000, 213.5000000000000000 ) ) ;
#8622 = CARTESIAN_POINT ( 'NONE',  ( -115.5625104412419972, 20.79694577648909615, -234.3927740977559893 ) ) ;
#8623 = DIRECTION ( 'NONE',  ( 0.000000000000000000, 1.000000000000000000, 0.000000000000000000 ) ) ;
#8624 = CARTESIAN_POINT ( 'NONE',  ( 0.000000000000000000, 0.000000000000000000, 0.000000000000000000 ) ) ;
#8625 = DIRECTION ( 'NONE',  ( 0.000000000000000000, 1.000000000000000000, 0.000000000000000000 ) ) ;
#8626 = CARTESIAN_POINT ( 'NONE',  ( -212.0849693193241592, 20.79694577634646535, 151.9741924115227789 ) ) ;
#8627 = MECHANICAL_DESIGN_GEOMETRIC_PRESENTATION_REPRESENTATION (  '', ( #9477 ), #8841 ) ;
#8628 = VERTEX_POINT ( 'NONE', #1224 ) ;
#8629 = CARTESIAN_POINT ( 'NONE',  ( 221.5672498511021331, 20.79694577634646890, -137.7829567244531006 ) ) ;
#8630 = ORIENTED_EDGE ( 'NONE', *, *, #10626, .F. ) ;
#8631 = DIRECTION ( 'NONE',  ( 0.000000000000000000, 0.000000000000000000, 1.000000000000000000 ) ) ;
#8632 = ORIENTED_EDGE ( 'NONE', *, *, #6958, .F. ) ;
#8633 = VERTEX_POINT ( 'NONE', #5284 ) ;
#8634 = VECTOR ( 'NONE', #12589, 1000.000000000000114 ) ;
#8635 = DIRECTION ( 'NONE',  ( 0.000000000000000000, -0.7071067811865489050, -0.7071067811865460184 ) ) ;
#8636 = FACE_OUTER_BOUND ( 'NONE', #2613, .T. ) ;
#8637 = CIRCLE ( 'NONE', #12674, 1.750000000000000000 ) ;
#8638 = DIRECTION ( 'NONE',  ( -0.000000000000000000, -1.000000000000000000, 0.000000000000000000 ) ) ;
#8639 = CARTESIAN_POINT ( 'NONE',  ( 159.3442861576696998, 0.000000000000000000, 192.8974817588416784 ) ) ;
#8640 =( NAMED_UNIT ( * ) PLANE_ANGLE_UNIT ( ) SI_UNIT ( $, .RADIAN. ) );
#8641 = FACE_BOUND ( 'NONE', #12052, .T. ) ;
#8642 = ORIENTED_EDGE ( 'NONE', *, *, #6698, .T. ) ;
#8643 = DIRECTION ( 'NONE',  ( 0.6368676505102707219, 0.000000000000000000, 0.7709731485165536302 ) ) ;
#8644 = CIRCLE ( 'NONE', #2879, 5.500000000000007994 ) ;
#8645 = ORIENTED_EDGE ( 'NONE', *, *, #1828, .T. ) ;
#8646 =( REPRESENTATION_RELATIONSHIP ('NONE','NONE', #12019, #182 ) REPRESENTATION_RELATIONSHIP_WITH_TRANSFORMATION ( #8514 )SHAPE_REPRESENTATION_RELATIONSHIP( ) );
#8647 = CARTESIAN_POINT ( 'NONE',  ( -241.0175249737202989, 4.851820797274892350, -10.70187039120737005 ) ) ;
#8648 = DIRECTION ( 'NONE',  ( 0.6368676505102700558, 0.000000000000000000, 0.7709731485165541853 ) ) ;
#8649 = EDGE_CURVE ( 'NONE', #5629, #1965, #8782, .T. ) ;
#8650 = EDGE_CURVE ( 'NONE', #4613, #1970, #3451, .T. ) ;
#8651 = DIRECTION ( 'NONE',  ( -0.000000000000000000, -1.000000000000000000, 0.000000000000000000 ) ) ;
#8652 = CARTESIAN_POINT ( 'NONE',  ( -239.4758390117360989, 1.805333157548462131, 11.86347296100405124 ) ) ;
#8653 = CARTESIAN_POINT ( 'NONE',  ( -229.7304563602428402, 3.778965902296226975, 11.13238168007022288 ) ) ;
#8654 = CARTESIAN_POINT ( 'NONE',  ( -246.5457465981856160, -9.425397935063502430, 7.427386666392754577 ) ) ;
#8655 = LINE ( 'NONE', #11659, #10327 ) ;
#8656 = CARTESIAN_POINT ( 'NONE',  ( -229.9035215981751890, 9.983406791829001037, 6.668687660899911052 ) ) ;
#8657 = ORIENTED_EDGE ( 'NONE', *, *, #6048, .T. ) ;
#8658 = DIRECTION ( 'NONE',  ( 0.000000000000000000, 1.000000000000000000, 0.000000000000000000 ) ) ;
#8659 = ORIENTED_EDGE ( 'NONE', *, *, #1603, .T. ) ;
#8660 = CARTESIAN_POINT ( 'NONE',  ( 234.7354397751814759, 19.96883746015188876, -115.7315435904363312 ) ) ;
#8661 = CARTESIAN_POINT ( 'NONE',  ( 153.9282213272189495, -18.00000000000000000, 245.7765299597151341 ) ) ;
#8662 = FACE_OUTER_BOUND ( 'NONE', #11960, .T. ) ;
#8663 = CARTESIAN_POINT ( 'NONE',  ( -241.2864786002318453, 5.310083909468028551, 10.76118394184098825 ) ) ;
#8664 = DIRECTION ( 'NONE',  ( 0.000000000000000000, 0.000000000000000000, -1.000000000000000000 ) ) ;
#8665 = DIRECTION ( 'NONE',  ( -0.7545873610930038389, 0.5538822189107471816, 0.3518698652246366465 ) ) ;
#8666 = EDGE_CURVE ( 'NONE', #3345, #11715, #12550, .T. ) ;
#8667 = CARTESIAN_POINT ( 'NONE',  ( 229.9733680233429993, 8.492964294626340574E-17, 3.499999999999964917 ) ) ;
#8668 = ITEM_DEFINED_TRANSFORMATION ( 'NONE', 'NONE', #6581,  #805 ) ;
#8669 = ADVANCED_FACE ( 'NONE', ( #2418 ), #10059, .F. ) ;
#8670 = CARTESIAN_POINT ( 'NONE',  ( -241.4352517270689589, -5.538320168158482382, -10.64816312893004202 ) ) ;
#8671 = VECTOR ( 'NONE', #1865, 1000.000000000000114 ) ;
#8672 = CARTESIAN_POINT ( 'NONE',  ( 1.104728353688762803E-12, 19.96883746059272724, -261.1558126970361400 ) ) ;
#8673 = ORIENTED_EDGE ( 'NONE', *, *, #4371, .T. ) ;
#8674 = EDGE_LOOP ( 'NONE', ( #11117, #4623, #9741, #7718 ) ) ;
#8675 = LINE ( 'NONE', #4598, #4630 ) ;
#8676 = CARTESIAN_POINT ( 'NONE',  ( 122.2593324768334071, 19.00000000000000000, -173.7755348299895104 ) ) ;
#8677 = CARTESIAN_POINT ( 'NONE',  ( 159.4136521832723474, 20.55460285070720161, -207.7919029841772840 ) ) ;
#8678 = CARTESIAN_POINT ( 'NONE',  ( 229.2637990951503753, -18.00000000000000000, -180.9540284836414514 ) ) ;
#8679 = DIRECTION ( 'NONE',  ( -0.7071067811865512365, 0.000000000000000000, 0.7071067811865437980 ) ) ;
#8680 = DIRECTION ( 'NONE',  ( 0.000000000000000000, 0.000000000000000000, 1.000000000000000000 ) ) ;
#8681 = DIRECTION ( 'NONE',  ( 0.000000000000000000, 1.000000000000000000, 0.000000000000000000 ) ) ;
#8682 = EDGE_CURVE ( 'NONE', #4419, #1170, #10260, .T. ) ;
#8683 = ORIENTED_EDGE ( 'NONE', *, *, #9319, .T. ) ;
#8684 = CARTESIAN_POINT ( 'NONE',  ( 8.533827019709857353, 20.79694577634646535, -260.7745447061712980 ) ) ;
#8685 = VERTEX_POINT ( 'NONE', #12428 ) ;
#8686 = DIRECTION ( 'NONE',  ( 0.000000000000000000, 1.000000000000000000, 0.000000000000000000 ) ) ;
#8687 = ORIENTED_EDGE ( 'NONE', *, *, #6407, .T. ) ;
#8688 = ORIENTED_EDGE ( 'NONE', *, *, #2555, .T. ) ;
#8689 = AXIS2_PLACEMENT_3D ( 'NONE', #686, #1819, #5750 ) ;
#8690 = ORIENTED_EDGE ( 'NONE', *, *, #7100, .T. ) ;
#8691 = DIRECTION ( 'NONE',  ( -0.000000000000000000, -1.000000000000000000, 0.000000000000000000 ) ) ;
#8692 = CARTESIAN_POINT ( 'NONE',  ( -293.0608542803120145, -28.60000000000000142, 6.485521991431944855 ) ) ;
#8693 = CARTESIAN_POINT ( 'NONE',  ( 67.55708173896789503, 20.08915143276009729, -252.2208631674930359 ) ) ;
#8694 = DIRECTION ( 'NONE',  ( 0.000000000000000000, 0.000000000000000000, 1.000000000000000000 ) ) ;
#8695 = DIRECTION ( 'NONE',  ( -1.000000000000000000, -0.000000000000000000, -0.000000000000000000 ) ) ;
#8696 = DIRECTION ( 'NONE',  ( 0.000000000000000000, 0.000000000000000000, 1.000000000000000000 ) ) ;
#8697 = CIRCLE ( 'NONE', #2938, 2.000000000000000444 ) ;
#8698 = CIRCLE ( 'NONE', #12108, 5.500000000000005329 ) ;
#8699 = ITEM_DEFINED_TRANSFORMATION ( 'NONE', 'NONE', #1667,  #805 ) ;
#8700 = ORIENTED_EDGE ( 'NONE', *, *, #7099, .F. ) ;
#8701 = AXIS2_PLACEMENT_3D ( 'NONE', #12814, #8686, #367 ) ;
#8702 = DIRECTION ( 'NONE',  ( -0.000000000000000000, 1.000000000000000000, 0.000000000000000000 ) ) ;
#8703 = CONICAL_SURFACE ( 'NONE', #4443, 249.0000000000000284, 1.373400766945015894 ) ;
#8704 = ORIENTED_EDGE ( 'NONE', *, *, #10314, .F. ) ;
#8705 = CARTESIAN_POINT ( 'NONE',  ( -244.6749594661061167, 8.549245787831393883, -8.062606910321274967 ) ) ;
#8706 = ORIENTED_EDGE ( 'NONE', *, *, #7951, .F. ) ;
#8707 = VECTOR ( 'NONE', #10658, 1000.000000000000000 ) ;
#8708 = AXIS2_PLACEMENT_3D ( 'NONE', #11464, #3318, #8535 ) ;
#8709 = CONICAL_SURFACE ( 'NONE', #11284, 304.0000000000000000, 0.7853981633974207455 ) ;
#8710 = CARTESIAN_POINT ( 'NONE',  ( 240.2816503055146882, -2.505215826205224872, -2.444791323730728827 ) ) ;
#8711 = CARTESIAN_POINT ( 'NONE',  ( -122.2593324768359935, 30.00000000000000000, -161.7755348299880040 ) ) ;
#8712 = DIRECTION ( 'NONE',  ( -0.000000000000000000, -1.000000000000000000, 0.000000000000000000 ) ) ;
#8713 = DIRECTION ( 'NONE',  ( -1.000000000000000000, 0.000000000000000000, 0.000000000000000000 ) ) ;
#8714 = AXIS2_PLACEMENT_3D ( 'NONE', #2236, #7307, #9305 ) ;
#8715 = DIRECTION ( 'NONE',  ( 0.000000000000000000, 0.9998057603070481525, -0.01970892327970899874 ) ) ;
#8716 = DIRECTION ( 'NONE',  ( 0.000000000000000000, -1.000000000000000000, 0.000000000000000000 ) ) ;
#8717 = CONTEXT_DEPENDENT_SHAPE_REPRESENTATION ( #5740, #6511 ) ;
#8718 =( REPRESENTATION_RELATIONSHIP ('NONE','NONE', #12019, #8443 ) REPRESENTATION_RELATIONSHIP_WITH_TRANSFORMATION ( #4706 )SHAPE_REPRESENTATION_RELATIONSHIP( ) );
#8719 = ADVANCED_FACE ( 'NONE', ( #424 ), #10489, .F. ) ;
#8720 = CARTESIAN_POINT ( 'NONE',  ( -229.9210428544502065, 10.37906049596799463, 6.034458640445298450 ) ) ;
#8721 = ADVANCED_FACE ( 'NONE', ( #12485 ), #9360, .F. ) ;
#8722 = VECTOR ( 'NONE', #6015, 1000.000000000000114 ) ;
#8723 = ORIENTED_EDGE ( 'NONE', *, *, #7224, .F. ) ;
#8724 = CIRCLE ( 'NONE', #34, 4.000000000000000000 ) ;
#8725 = EDGE_LOOP ( 'NONE', ( #1594, #6814 ) ) ;
#8726 = CARTESIAN_POINT ( 'NONE',  ( -248.9051445895378833, -10.17462340911300522, -5.878044170152538328 ) ) ;
#8727 = EDGE_LOOP ( 'NONE', ( #434, #5627, #5686, #1987, #2491, #7920, #3271, #1620, #8853, #5294 ) ) ;
#8728 = CARTESIAN_POINT ( 'NONE',  ( -17.09264059789343193, 19.96883746059643983, -261.1558126970361400 ) ) ;
#8729 = DIRECTION ( 'NONE',  ( -0.6368676505102689456, 0.000000000000000000, -0.7709731485165549625 ) ) ;
#8730 = LINE ( 'NONE', #6932, #1253 ) ;
#8731 = CARTESIAN_POINT ( 'NONE',  ( 197.8197553893920144, 29.00000000000000000, 58.77553482998850853 ) ) ;
#8732 = AXIS2_PLACEMENT_3D ( 'NONE', #11608, #6410, #6607 ) ;
#8733 = CARTESIAN_POINT ( 'NONE',  ( -239.9867712987591801, -2.433335514368112129, 11.49559079283389096 ) ) ;
#8734 = CARTESIAN_POINT ( 'NONE',  ( 294.8238222686200061, -30.00000000000000000, 32.70078231946946090 ) ) ;
#8735 = DIRECTION ( 'NONE',  ( -0.9396926207859104263, 0.000000000000000000, 0.3420201433256630508 ) ) ;
#8736 = CARTESIAN_POINT ( 'NONE',  ( -229.7036025737252203, -1.539969265571519363, -11.67378731463722019 ) ) ;
#8737 = AXIS2_PLACEMENT_3D ( 'NONE', #10666, #12671, #1669 ) ;
#8738 = CARTESIAN_POINT ( 'NONE',  ( -249.7276455219525815, 11.33491751851197549, 3.110604576379348174 ) ) ;
#8739 = DIRECTION ( 'NONE',  ( 0.000000000000000000, 1.000000000000000000, 0.000000000000000000 ) ) ;
#8740 = CARTESIAN_POINT ( 'NONE',  ( -229.8178335282108264, -7.766306225721687717, 9.155633550835144518 ) ) ;
#8741 = ORIENTED_EDGE ( 'NONE', *, *, #9805, .F. ) ;
#8742 = ORIENTED_EDGE ( 'NONE', *, *, #6649, .T. ) ;
#8743 = CARTESIAN_POINT ( 'NONE',  ( 0.000000000000000000, -20.00000000000000000, 0.000000000000000000 ) ) ;
#8744 = CARTESIAN_POINT ( 'NONE',  ( 227.3999999999999773, 4.447920636657316074, -2.686261716586451520 ) ) ;
#8745 = EDGE_CURVE ( 'NONE', #11239, #11433, #1765, .T. ) ;
#8746 = EDGE_CURVE ( 'NONE', #4210, #6668, #164, .T. ) ;
#8747 = CARTESIAN_POINT ( 'NONE',  ( -247.4557548106230058, 20.79694577606145600, -84.02568524181840814 ) ) ;
#8748 = DIRECTION ( 'NONE',  ( 0.000000000000000000, 1.000000000000000000, 0.000000000000000000 ) ) ;
#8749 = CARTESIAN_POINT ( 'NONE',  ( 0.000000000000000000, 0.000000000000000000, 0.000000000000000000 ) ) ;
#8750 = DIRECTION ( 'NONE',  ( 0.000000000000000000, 1.000000000000000000, 0.000000000000000000 ) ) ;
#8751 = FACE_BOUND ( 'NONE', #9238, .T. ) ;
#8752 = VERTEX_POINT ( 'NONE', #10491 ) ;
#8753 = DIRECTION ( 'NONE',  ( -0.4503334343941818307, -0.7071067811865080488, -0.5451603414288285210 ) ) ;
#8754 = EDGE_LOOP ( 'NONE', ( #144, #4799, #7223, #6326 ) ) ;
#8755 = VERTEX_POINT ( 'NONE', #8301 ) ;
#8756 = CIRCLE ( 'NONE', #40, 254.1999999999999886 ) ;
#8757 = CARTESIAN_POINT ( 'NONE',  ( 130.3442252640560639, 20.08915143297736705, 225.7689075324037731 ) ) ;
#8758 = EDGE_LOOP ( 'NONE', ( #7973, #9035, #10770, #2381 ) ) ;
#8759 = CARTESIAN_POINT ( 'NONE',  ( 227.3999999999999773, -4.550331206106116078, -2.508881407069070590 ) ) ;
#8760 = ORIENTED_EDGE ( 'NONE', *, *, #11124, .F. ) ;
#8761 = ADVANCED_FACE ( 'NONE', ( #5358 ), #3214, .T. ) ;
#8762 = CARTESIAN_POINT ( 'NONE',  ( 235.4000000000000057, 0.1024105694487990881, 5.195143123655512341 ) ) ;
#8763 = CARTESIAN_POINT ( 'NONE',  ( -67.55708173894439028, 20.08915143292001204, -252.2208631666825056 ) ) ;
#8764 = CARTESIAN_POINT ( 'NONE',  ( -122.2593324768321992, 30.00000000000000000, 168.2755348299905052 ) ) ;
#8765 =( NAMED_UNIT ( * ) PLANE_ANGLE_UNIT ( ) SI_UNIT ( $, .RADIAN. ) );
#8766 = CARTESIAN_POINT ( 'NONE',  ( 3.053044470274351535E-14, 25.00000000000000000, -249.2999999999999829 ) ) ;
#8767 = ADVANCED_FACE ( 'NONE', ( #359 ), #10285, .F. ) ;
#8768 = VERTEX_POINT ( 'NONE', #4473 ) ;
#8769 = CARTESIAN_POINT ( 'NONE',  ( -159.3442861576696998, 11.79660968244693997, -192.8974817588416784 ) ) ;
#8770 = VERTEX_POINT ( 'NONE', #8557 ) ;
#8771 = PRODUCT_DEFINITION_SHAPE ( 'NONE', 'NONE',  #13182 ) ;
#8772 = CARTESIAN_POINT ( 'NONE',  ( -243.1145437067741852, 7.410518231008048851, -9.118492838939154410 ) ) ;
#8773 = ORIENTED_EDGE ( 'NONE', *, *, #12004, .T. ) ;
#8774 = AXIS2_PLACEMENT_3D ( 'NONE', #3529, #7539, #1108 ) ;
#8775 = LINE ( 'NONE', #3709, #10033 ) ;
#8776 = CARTESIAN_POINT ( 'NONE',  ( 122.2593324768334071, 30.00000000000000000, -174.7755348299895104 ) ) ;
#8777 = FACE_OUTER_BOUND ( 'NONE', #6927, .T. ) ;
#8778 = VECTOR ( 'NONE', #9797, 1000.000000000000000 ) ;
#8779 = CARTESIAN_POINT ( 'NONE',  ( 3.010181832304193602E-14, 0.000000000000000000, 245.7999999999999829 ) ) ;
#8780 = PRODUCT_DEFINITION_SHAPE ( 'NONE', 'NONE',  #13109 ) ;
#8781 = CARTESIAN_POINT ( 'NONE',  ( -243.5834864928896195, -7.809424032089201440, 9.110990436359818645 ) ) ;
#8782 = CIRCLE ( 'NONE', #1116, 249.7999999999999829 ) ;
#8783 = CARTESIAN_POINT ( 'NONE',  ( -0.000000000000000000, -21.50000000000000000, 0.000000000000000000 ) ) ;
#8784 = ORIENTED_EDGE ( 'NONE', *, *, #12515, .T. ) ;
#8785 = AXIS2_PLACEMENT_3D ( 'NONE', #1102, #6111, #5240 ) ;
#8786 = CARTESIAN_POINT ( 'NONE',  ( -165.3358371128624924, 2.772967769358929857, -200.1506762031210371 ) ) ;
#8787 = ORIENTED_EDGE ( 'NONE', *, *, #5179, .T. ) ;
#8788 = ORIENTED_EDGE ( 'NONE', *, *, #8004, .F. ) ;
#8789 = DIRECTION ( 'NONE',  ( -0.000000000000000000, -1.000000000000000000, 0.000000000000000000 ) ) ;
#8790 = EDGE_LOOP ( 'NONE', ( #4293, #10573, #2130, #2064 ) ) ;
#8791 = AXIS2_PLACEMENT_3D ( 'NONE', #4269, #10269, #7402 ) ;
#8792 = CARTESIAN_POINT ( 'NONE',  ( 261.3381329044966606, 20.55460285106647689, -17.10461161501038063 ) ) ;
#8793 = CARTESIAN_POINT ( 'NONE',  ( -122.2593324768321992, 30.00000000000000000, 174.7755348299905052 ) ) ;
#8794 = DIRECTION ( 'NONE',  ( -0.000000000000000000, -1.000000000000000000, 0.000000000000000000 ) ) ;
#8795 = EDGE_CURVE ( 'NONE', #12496, #534, #12615, .T. ) ;
#8796 = FACE_OUTER_BOUND ( 'NONE', #10999, .T. ) ;
#8797 = DIRECTION ( 'NONE',  ( 8.659560562355171982E-17, 0.7071067811865280328, -0.7071067811865670016 ) ) ;
#8798 = DIRECTION ( 'NONE',  ( 0.000000000000000000, -1.000000000000000000, 0.000000000000000000 ) ) ;
#8799 = CARTESIAN_POINT ( 'NONE',  ( -32.05991134143113186, -138.4705547276867321, -26.90145978217142542 ) ) ;
#8800 = VECTOR ( 'NONE', #5764, 1000.000000000000000 ) ;
#8801 = CARTESIAN_POINT ( 'NONE',  ( -229.9800961966465707, -11.35427705715375168, -3.048062575764186821 ) ) ;
#8802 = VECTOR ( 'NONE', #2901, 1000.000000000000000 ) ;
#8803 = CONICAL_SURFACE ( 'NONE', #12218, 5.500000000000005329, 0.7853981633974461696 ) ;
#8804 = CARTESIAN_POINT ( 'NONE',  ( -249.3500139047057473, 10.59807002901562001, -5.074486595297502234 ) ) ;
#8805 = CARTESIAN_POINT ( 'NONE',  ( -240.7195678457707402, -4.326096554271789074, -11.19626641913139409 ) ) ;
#8806 = CARTESIAN_POINT ( 'NONE',  ( -229.8758178857063399, -9.335232842866593828, -7.576971754760646327 ) ) ;
#8807 = EDGE_LOOP ( 'NONE', ( #3206, #3977, #10295, #5791 ) ) ;
#8808 = EDGE_LOOP ( 'NONE', ( #7395, #7353, #2977, #2722 ) ) ;
#8809 = DIRECTION ( 'NONE',  ( 0.000000000000000000, 1.000000000000000000, 0.000000000000000000 ) ) ;
#8810 = CARTESIAN_POINT ( 'NONE',  ( 0.000000000000000000, 0.000000000000000000, -245.7999999999999829 ) ) ;
#8811 = ADVANCED_FACE ( 'NONE', ( #11626 ), #5379, .T. ) ;
#8812 = EDGE_CURVE ( 'NONE', #11730, #7406, #226, .T. ) ;
#8813 = PRODUCT_DEFINITION_SHAPE ( 'NONE', 'NONE',  #13044 ) ;
#8814 = AXIS2_PLACEMENT_3D ( 'NONE', #8407, #4390, #10467 ) ;
#8815 = CARTESIAN_POINT ( 'NONE',  ( -260.7745447066434963, 20.79694577614318618, -17.06760680913714978 ) ) ;
#8816 = DIRECTION ( 'NONE',  ( 1.000000000000000000, 0.000000000000000000, 0.000000000000000000 ) ) ;
#8817 = DIRECTION ( 'NONE',  ( -0.7660444431189726844, 0.000000000000000000, -0.6427876096865458022 ) ) ;
#8818 = FACE_OUTER_BOUND ( 'NONE', #6205, .T. ) ;
#8819 = CARTESIAN_POINT ( 'NONE',  ( 240.2701176883045093, 2.464548987102257449, -2.493043655922373425 ) ) ;
#8820 = VERTEX_POINT ( 'NONE', #8678 ) ;
#8821 = EDGE_CURVE ( 'NONE', #1614, #5331, #12823, .T. ) ;
#8822 = AXIS2_PLACEMENT_3D ( 'NONE', #148, #12532, #5405 ) ;
#8823 = CARTESIAN_POINT ( 'NONE',  ( -238.8090076327945894, -0.7315829084426003215, 11.97771329485296299 ) ) ;
#8824 = ORIENTED_EDGE ( 'NONE', *, *, #6081, .T. ) ;
#8825 = VERTEX_POINT ( 'NONE', #1551 ) ;
#8826 = CARTESIAN_POINT ( 'NONE',  ( 233.8077470125390676, 20.08915143297735995, -115.3046144132253374 ) ) ;
#8827 = ORIENTED_EDGE ( 'NONE', *, *, #5254, .T. ) ;
#8828 = CARTESIAN_POINT ( 'NONE',  ( 197.8197553893915028, 18.00000000000000000, -70.77553482998990830 ) ) ;
#8829 = CARTESIAN_POINT ( 'NONE',  ( 239.0281511860549699, -0.5135531387677250148, -3.462181616333541712 ) ) ;
#8830 = CARTESIAN_POINT ( 'NONE',  ( -258.8746690723625079, 20.08915143294039396, -34.10614053585524630 ) ) ;
#8831 = AXIS2_PLACEMENT_3D ( 'NONE', #2836, #1791, #8051 ) ;
#8832 = DIRECTION ( 'NONE',  ( 0.000000000000000000, 0.000000000000000000, -1.000000000000000000 ) ) ;
#8833 =( NAMED_UNIT ( * ) PLANE_ANGLE_UNIT ( ) SI_UNIT ( $, .RADIAN. ) );
#8834 = ORIENTED_EDGE ( 'NONE', *, *, #5052, .T. ) ;
#8835 = CARTESIAN_POINT ( 'NONE',  ( 220.3999999999999773, 0.000000000000000000, 0.000000000000000000 ) ) ;
#8836 = ADVANCED_FACE ( 'NONE', ( #6693 ), #10692, .F. ) ;
#8837 = ORIENTED_EDGE ( 'NONE', *, *, #2881, .F. ) ;
#8838 = EDGE_CURVE ( 'NONE', #12848, #2425, #5831, .T. ) ;
#8839 = CARTESIAN_POINT ( 'NONE',  ( -238.9707249590438494, 1.103996713823099496, 11.69802420356912087 ) ) ;
#8840 = ORIENTED_EDGE ( 'NONE', *, *, #9525, .T. ) ;
#8841 =( GEOMETRIC_REPRESENTATION_CONTEXT ( 3 ) GLOBAL_UNCERTAINTY_ASSIGNED_CONTEXT ( ( #6923 ) ) GLOBAL_UNIT_ASSIGNED_CONTEXT ( ( #2321, #333, #3377 ) ) REPRESENTATION_CONTEXT ( 'NONE', 'WORKASPACE' ) );
#8842 = VECTOR ( 'NONE', #1099, 1000.000000000000000 ) ;
#8843 = ADVANCED_FACE ( 'NONE', ( #5749 ), #11972, .F. ) ;
#8844 = DIRECTION ( 'NONE',  ( 0.000000000000000000, 0.000000000000000000, -1.000000000000000000 ) ) ;
#8845 = FACE_OUTER_BOUND ( 'NONE', #8440, .T. ) ;
#8846 = CARTESIAN_POINT ( 'NONE',  ( -249.7118339206215012, -9.997999799959989886, -6.636264009214830395 ) ) ;
#8847 = CARTESIAN_POINT ( 'NONE',  ( -229.7748312726236293, 5.886477795347762942, -10.17644301346884816 ) ) ;
#8848 = CARTESIAN_POINT ( 'NONE',  ( -196.0019244007923476, 20.08915143297736705, 171.8850263962750660 ) ) ;
#8849 = CARTESIAN_POINT ( 'NONE',  ( -244.9313462850813039, -8.700834631469609448, 8.264179333479736655 ) ) ;
#8850 = CONICAL_SURFACE ( 'NONE', #10121, 6.500000000000005329, 0.7853981633974476129 ) ;
#8851 = CARTESIAN_POINT ( 'NONE',  ( -239.5624944925539239, 1.883403902577551969, -11.85129291162959042 ) ) ;
#8852 =( REPRESENTATION_RELATIONSHIP ('NONE','NONE', #12019, #5191 ) REPRESENTATION_RELATIONSHIP_WITH_TRANSFORMATION ( #11535 )SHAPE_REPRESENTATION_RELATIONSHIP( ) );
#8853 = ORIENTED_EDGE ( 'NONE', *, *, #7767, .T. ) ;
#8854 = CARTESIAN_POINT ( 'NONE',  ( -229.8083007641753568, 7.475044586470752428, 9.389288305976632998 ) ) ;
#8855 = EDGE_LOOP ( 'NONE', ( #5894, #9026, #6373, #11016 ) ) ;
#8856 = ADVANCED_FACE ( 'NONE', ( #12878 ), #12403, .F. ) ;
#8857 = ORIENTED_EDGE ( 'NONE', *, *, #3823, .T. ) ;
#8858 = CARTESIAN_POINT ( 'NONE',  ( -248.7692280202239772, -10.08940167826270340, -6.022204372421657403 ) ) ;
#8859 = ORIENTED_EDGE ( 'NONE', *, *, #9731, .F. ) ;
#8860 = CARTESIAN_POINT ( 'NONE',  ( -34.20858920326337227, 20.55460285088512506, -259.6535381484778782 ) ) ;
#8861 = DIRECTION ( 'NONE',  ( 0.000000000000000000, 1.000000000000000000, 0.000000000000000000 ) ) ;
#8862 = CARTESIAN_POINT ( 'NONE',  ( -122.2593324768321992, 19.00000000000000000, 168.2755348299905052 ) ) ;
#8863 = DIRECTION ( 'NONE',  ( 0.000000000000000000, -1.000000000000000000, 0.000000000000000000 ) ) ;
#8864 = DIRECTION ( 'NONE',  ( 0.000000000000000000, -1.000000000000000000, 0.000000000000000000 ) ) ;
#8865 = CARTESIAN_POINT ( 'NONE',  ( 235.4000000000000057, 0.000000000000000000, 0.000000000000000000 ) ) ;
#8866 = DIRECTION ( 'NONE',  ( -0.07256543843575240238, 0.5538822189107470706, -0.8294267566935215052 ) ) ;
#8867 = CARTESIAN_POINT ( 'NONE',  ( 229.9902049636500863, 2.785755589373224428, 2.131144504211401891 ) ) ;
#8868 = CARTESIAN_POINT ( 'NONE',  ( -249.7994463212561982, 11.74985191749823699, 0.3872576247023094553 ) ) ;
#8869 = CARTESIAN_POINT ( 'NONE',  ( -247.8580199586201616, -9.788721918629967433, -6.941247868461743131 ) ) ;
#8870 = CARTESIAN_POINT ( 'NONE',  ( -230.0000048734746940, -12.00009112689273749, 0.1798068418026676774 ) ) ;
#8871 = ORIENTED_EDGE ( 'NONE', *, *, #7856, .F. ) ;
#8872 = ORIENTED_EDGE ( 'NONE', *, *, #1988, .T. ) ;
#8873 = DIRECTION ( 'NONE',  ( -0.000000000000000000, -1.000000000000000000, 0.000000000000000000 ) ) ;
#8874 = DIRECTION ( 'NONE',  ( -0.000000000000000000, -1.000000000000000000, 0.000000000000000000 ) ) ;
#8875 = CONICAL_SURFACE ( 'NONE', #7600, 5.499999999999998224, 0.7853981633974461696 ) ;
#8876 = CARTESIAN_POINT ( 'NONE',  ( -130.6873781523279945, 20.79694577633451402, 226.3083638767075172 ) ) ;
#8877 = DIRECTION ( 'NONE',  ( 0.000000000000000000, 1.000000000000000000, 0.000000000000000000 ) ) ;
#8878 = CARTESIAN_POINT ( 'NONE',  ( 0.000000000000000000, 0.000000000000000000, 0.000000000000000000 ) ) ;
#8879 = CARTESIAN_POINT ( 'NONE',  ( 71.82423009839129691, 30.00000000000000000, 197.3354503650404865 ) ) ;
#8880 = CARTESIAN_POINT ( 'NONE',  ( 240.3371538976029456, 2.621326596184952340, -2.332469087881691383 ) ) ;
#8881 = ORIENTED_EDGE ( 'NONE', *, *, #5666, .T. ) ;
#8882 = EDGE_CURVE ( 'NONE', #7690, #10052, #2178, .T. ) ;
#8883 = ADVANCED_FACE ( 'NONE', ( #9674 ), #268, .F. ) ;
#8884 = CYLINDRICAL_SURFACE ( 'NONE', #5722, 5.100000000000017408 ) ;
#8885 = EDGE_LOOP ( 'NONE', ( #6716, #2791, #4467, #11855 ) ) ;
#8886 = ORIENTED_EDGE ( 'NONE', *, *, #2074, .F. ) ;
#8887 = PRODUCT_DEFINITION_CONTEXT ( 'detailed design', #3002, 'design' ) ;
#8888 = DIRECTION ( 'NONE',  ( -0.5469441386039890496, 0.000000000000000000, 0.8371691043312220470 ) ) ;
#8889 = EDGE_LOOP ( 'NONE', ( #1204, #5974, #10971, #9933 ) ) ;
#8890 = PRODUCT_DEFINITION_SHAPE ( 'NONE', 'NONE',  #13120 ) ;
#8891 = DIRECTION ( 'NONE',  ( 1.000000000000000000, 0.000000000000000000, 0.000000000000000000 ) ) ;
#8892 = CIRCLE ( 'NONE', #3001, 5.499999999999986677 ) ;
#8893 = APPLICATION_CONTEXT ( 'automotive_design' ) ;
#8894 = EDGE_CURVE ( 'NONE', #5845, #10191, #3876, .T. ) ;
#8895 = CARTESIAN_POINT ( 'NONE',  ( -207.1687172310330141, 20.08915143305816997, -158.9353507251184965 ) ) ;
#8896 = CARTESIAN_POINT ( 'NONE',  ( 0.000000000000000000, 21.99999999999995381, 0.000000000000000000 ) ) ;
#8897 = DIRECTION ( 'NONE',  ( 8.659560562354693735E-17, 0.7071067811865670016, -0.7071067811865280328 ) ) ;
#8898 = ORIENTED_EDGE ( 'NONE', *, *, #3916, .T. ) ;
#8899 = DIRECTION ( 'NONE',  ( 0.6368676505102707219, 0.000000000000000000, 0.7709731485165536302 ) ) ;
#8901 = ORIENTED_EDGE ( 'NONE', *, *, #8106, .T. ) ;
#8900 = AXIS2_PLACEMENT_3D ( 'NONE', #11222, #7097, #3014 ) ;
#8902 = CARTESIAN_POINT ( 'NONE',  ( 0.000000000000000000, 21.50000000000000000, 0.000000000000000000 ) ) ;
#8903 = ORIENTED_EDGE ( 'NONE', *, *, #2512, .T. ) ;
#8904 = CARTESIAN_POINT ( 'NONE',  ( 3.034674768287141263E-14, -11.79660968244690089, -247.7999999999999829 ) ) ;
#8905 =( LENGTH_UNIT ( ) NAMED_UNIT ( * ) SI_UNIT ( .MILLI., .METRE. ) );
#8906 = CARTESIAN_POINT ( 'NONE',  ( -0.000000000000000000, -25.00000000000000000, 0.000000000000000000 ) ) ;
#8907 = CIRCLE ( 'NONE', #4220, 5.500000000000005329 ) ;
#8908 = CIRCLE ( 'NONE', #4221, 196.0000000000000000 ) ;
#8909 = ADVANCED_FACE ( 'NONE', ( #2606 ), #10615, .F. ) ;
#8910 = AXIS2_PLACEMENT_3D ( 'NONE', #9671, #10805, #6689 ) ;
#8911 = CARTESIAN_POINT ( 'NONE',  ( -238.6985546646470198, 6.516754929249349828E-09, -12.00000000011316459 ) ) ;
#8912 = CONICAL_SURFACE ( 'NONE', #2716, 249.7999999999999829, 0.7853981633974066456 ) ;
#8913 = AXIS2_PLACEMENT_3D ( 'NONE', #4074, #9080, #10077 ) ;
#8914 = EDGE_CURVE ( 'NONE', #12886, #11448, #11122, .T. ) ;
#8915 = CARTESIAN_POINT ( 'NONE',  ( -251.8100110699623144, 20.08915143297736705, -67.47543992452018813 ) ) ;
#8916 = AXIS2_PLACEMENT_3D ( 'NONE', #9419, #7285, #6292 ) ;
#8917 = CARTESIAN_POINT ( 'NONE',  ( -241.6004288479487343, -5.767183905185619963, 10.52387470033283812 ) ) ;
#8918 = CARTESIAN_POINT ( 'NONE',  ( -130.4544329367265902, 20.79694577634646535, -225.9597979674047110 ) ) ;
#8919 = ORIENTED_EDGE ( 'NONE', *, *, #1899, .T. ) ;
#8920 = CARTESIAN_POINT ( 'NONE',  ( -238.9571479262659750, -1.076402584257635686, -11.70061130326932464 ) ) ;
#8921 = ORIENTED_EDGE ( 'NONE', *, *, #12278, .T. ) ;
#8922 = PRODUCT_DEFINITION_SHAPE ( 'NONE', 'NONE',  #13080 ) ;
#8923 = ORIENTED_EDGE ( 'NONE', *, *, #2036, .T. ) ;
#8924 = VECTOR ( 'NONE', #10992, 1000.000000000000114 ) ;
#8925 = CARTESIAN_POINT ( 'NONE',  ( -249.7762712555648932, -11.55521436350650255, -2.133810497648569893 ) ) ;
#8926 = ORIENTED_EDGE ( 'NONE', *, *, #12032, .T. ) ;
#8927 = CARTESIAN_POINT ( 'NONE',  ( 115.8123742910162264, 20.55460285096275541, -234.8993005738286115 ) ) ;
#8928 = EDGE_CURVE ( 'NONE', #10624, #10245, #7818, .T. ) ;
#8929 = CARTESIAN_POINT ( 'NONE',  ( 171.9542656377731191, -18.00000000000000000, 208.1627500994694628 ) ) ;
#8930 =( GEOMETRIC_REPRESENTATION_CONTEXT ( 3 ) GLOBAL_UNCERTAINTY_ASSIGNED_CONTEXT ( ( #12169 ) ) GLOBAL_UNIT_ASSIGNED_CONTEXT ( ( #313, #1176, #2098 ) ) REPRESENTATION_CONTEXT ( 'NONE', 'WORKASPACE' ) );
#8931 = SPHERICAL_SURFACE ( 'NONE', #6369, 10.00000000000000000 ) ;
#8932 = TOROIDAL_SURFACE ( 'NONE', #12747, 258.5000000000000000, 2.500000000000035083 ) ;
#8933 = CARTESIAN_POINT ( 'NONE',  ( -294.8238222686198355, -30.00000000000000000, -32.70078231947154279 ) ) ;
#8934 = EDGE_CURVE ( 'NONE', #12854, #1691, #9004, .T. ) ;
#8935 = CARTESIAN_POINT ( 'NONE',  ( -239.9450917581424960, 2.156506209390990136, 11.80463811257499884 ) ) ;
#8936 = AXIS2_PLACEMENT_3D ( 'NONE', #2694, #8712, #5779 ) ;
#8937 = FACE_OUTER_BOUND ( 'NONE', #8306, .T. ) ;
#8938 = DIRECTION ( 'NONE',  ( -0.9063077870366523792, 0.000000000000000000, 0.4226182617406942787 ) ) ;
#8939 = CARTESIAN_POINT ( 'NONE',  ( -229.8892649129228971, -9.344369417327452965, 7.164599271245471357 ) ) ;
#8940 = EDGE_CURVE ( 'NONE', #3345, #8768, #10502, .T. ) ;
#8941 = CONTEXT_DEPENDENT_SHAPE_REPRESENTATION ( #1476, #7092 ) ;
#8942 = CARTESIAN_POINT ( 'NONE',  ( -249.7841416269946535, 11.60584252726589938, 1.834925605678527027 ) ) ;
#8943 = CARTESIAN_POINT ( 'NONE',  ( -220.9845196385168435, -30.00000000000000000, 190.9766794143566528 ) ) ;
#8944 = EDGE_LOOP ( 'NONE', ( #12803, #9219, #11764, #2155 ) ) ;
#8945 = VERTEX_POINT ( 'NONE', #4602 ) ;
#8946 = AXIS2_PLACEMENT_3D ( 'NONE', #8279, #9206, #3323 ) ;
#8947 = CARTESIAN_POINT ( 'NONE',  ( 228.6269314446401211, -30.00000000000000000, -181.7250016321579835 ) ) ;
#8948 = CARTESIAN_POINT ( 'NONE',  ( 197.8197553893920144, 19.00000000000000000, 69.77553482998851564 ) ) ;
#8949 = CARTESIAN_POINT ( 'NONE',  ( 67.61424743078299571, 20.79694577590440119, 252.4341100442090067 ) ) ;
#8950 = LINE ( 'NONE', #9015, #3463 ) ;
#8951 = DIRECTION ( 'NONE',  ( -0.9848077530122070211, 0.000000000000000000, -0.1736481776669374921 ) ) ;
#8952 = CARTESIAN_POINT ( 'NONE',  ( -245.3311829420961487, -8.905423748641078774, 7.665289358291517807 ) ) ;
#8953 = ORIENTED_EDGE ( 'NONE', *, *, #3863, .T. ) ;
#8954 = CYLINDRICAL_SURFACE ( 'NONE', #4028, 1.750000000000000000 ) ;
#8955 = AXIS2_PLACEMENT_3D ( 'NONE', #11128, #6006, #10064 ) ;
#8956 = CARTESIAN_POINT ( 'NONE',  ( -239.4323407727675885, -1.761903427608783046, 11.86994927914708242 ) ) ;
#8957 = ORIENTED_EDGE ( 'NONE', *, *, #10605, .T. ) ;
#8958 = ORIENTED_EDGE ( 'NONE', *, *, #2934, .T. ) ;
#8959 = CARTESIAN_POINT ( 'NONE',  ( 235.0999999999999943, 0.000000000000000000, 0.000000000000000000 ) ) ;
#8960 = EDGE_LOOP ( 'NONE', ( #6705, #11068, #9025, #382 ) ) ;
#8961 = AXIS2_PLACEMENT_3D ( 'NONE', #5671, #10800, #4659 ) ;
#8962 = DIRECTION ( 'NONE',  ( 0.000000000000000000, 0.000000000000000000, 1.000000000000000000 ) ) ;
#8963 = ADVANCED_FACE ( 'NONE', ( #12683 ), #3245, .F. ) ;
#8964 = CARTESIAN_POINT ( 'NONE',  ( -252.2208631657525473, 20.08915143310922957, 67.55708173876999467 ) ) ;
#8965 = CARTESIAN_POINT ( 'NONE',  ( -243.1520458356093286, -7.443371746667396316, 9.091683909978234723 ) ) ;
#8966 = LINE ( 'NONE', #11023, #1540 ) ;
#8967 = DIRECTION ( 'NONE',  ( -0.000000000000000000, -1.000000000000000000, 0.000000000000000000 ) ) ;
#8968 = ORIENTED_EDGE ( 'NONE', *, *, #11588, .F. ) ;
#8969 = CARTESIAN_POINT ( 'NONE',  ( 225.1241593668336236, -19.00000000000000000, -185.9653539489990521 ) ) ;
#8970 = ORIENTED_EDGE ( 'NONE', *, *, #8210, .T. ) ;
#8971 = CARTESIAN_POINT ( 'NONE',  ( -246.6693634553872982, 9.463199073315145426, -6.964939579051701024 ) ) ;
#8972 = EDGE_LOOP ( 'NONE', ( #7315, #11569, #8311, #8102 ) ) ;
#8973 = TOROIDAL_SURFACE ( 'NONE', #9596, 250.0000000000000000, 10.00000000000000000 ) ;
#8974 = CARTESIAN_POINT ( 'NONE',  ( 0.000000000000000000, 0.000000000000000000, 0.000000000000000000 ) ) ;
#8975 = CARTESIAN_POINT ( 'NONE',  ( 185.9653539490014111, -30.00000000000000000, 225.1241593668316625 ) ) ;
#8976 = DIRECTION ( 'NONE',  ( 0.000000000000000000, -1.000000000000000000, 0.000000000000000000 ) ) ;
#8977 = CARTESIAN_POINT ( 'NONE',  ( -249.7834747117780125, -11.65132285575867499, 2.887446915639924949 ) ) ;
#8978 = EDGE_CURVE ( 'NONE', #10501, #9249, #5548, .T. ) ;
#8979 = CARTESIAN_POINT ( 'NONE',  ( -229.9257603561380847, 10.20286607437010495, -5.878144477166547865 ) ) ;
#8980 = CARTESIAN_POINT ( 'NONE',  ( -67.47543992452052919, 20.08915143297736705, 251.8100110699622576 ) ) ;
#8981 = CARTESIAN_POINT ( 'NONE',  ( -240.5462192425719365, -3.949737371913570438, 11.33143176610938418 ) ) ;
#8982 = CARTESIAN_POINT ( 'NONE',  ( -190.4297758776777130, 20.79694577634646535, -178.3611219674585584 ) ) ;
#8983 = CONTEXT_DEPENDENT_SHAPE_REPRESENTATION ( #3432, #5719 ) ;
#8984 = EDGE_LOOP ( 'NONE', ( #322, #1033, #7531, #7918 ) ) ;
#8985 = CARTESIAN_POINT ( 'NONE',  ( -239.5361044668159991, -1.848645179572815156, -11.60366368868215758 ) ) ;
#8986 = ORIENTED_EDGE ( 'NONE', *, *, #9125, .F. ) ;
#8987 = ADVANCED_FACE ( 'NONE', ( #7806 ), #9224, .F. ) ;
#8988 = ORIENTED_EDGE ( 'NONE', *, *, #1514, .T. ) ;
#8989 = B_SPLINE_CURVE_WITH_KNOTS ( 'NONE', 3,
 ( #4496, #2686, #12641, #1578, #11646, #3501, #2500, #12701, #6583, #10638, #11714, #6646, #5640, #11096, #2819, #10970, #8034, #12165, #4959, #10032, #7480, #7036, #7102, #11026 ),
 .UNSPECIFIED., .F., .F.,
 ( 4, 2, 2, 1, 1, 2, 2, 2, 2, 1, 1, 2, 2, 4 ),
 ( 0.5000762939474624469, 0.6250572204606649196, 0.6875476837172660449, 0.7187929153455667741, 0.7344155311597135860, 0.7422268390667906557, 0.7500381469738676143, 0.8125286102304378755, 0.8437738418587181766, 0.8593964576728634341, 0.8672077655799359519, 0.8711134195334776509, 0.8750190734870191278, 1.000000000000000000 ),
 .UNSPECIFIED. ) ;
#8990 = EDGE_CURVE ( 'NONE', #3329, #11853, #1549, .T. ) ;
#8991 = CARTESIAN_POINT ( 'NONE',  ( -249.7843163504504389, -11.60707272974070214, -1.827122155921521607 ) ) ;
#8992 = ORIENTED_EDGE ( 'NONE', *, *, #4996, .T. ) ;
#8993 = AXIS2_PLACEMENT_3D ( 'NONE', #2063, #8141, #9133 ) ;
#8994 = CARTESIAN_POINT ( 'NONE',  ( 207.7919029858380213, 20.55460285149987953, -159.4136521842188188 ) ) ;
#8995 = CARTESIAN_POINT ( 'NONE',  ( -248.9599100168424286, 9.954851740884455680, -6.700860962377057639 ) ) ;
#8996 = DIRECTION ( 'NONE',  ( 0.000000000000000000, -0.9998057603070481525, 0.01970892327970899874 ) ) ;
#8997 = AXIS2_PLACEMENT_3D ( 'NONE', #8100, #2950, #12092 ) ;
#8998 = CARTESIAN_POINT ( 'NONE',  ( 0.000000000000000000, 0.000000000000000000, 0.000000000000000000 ) ) ;
#8999 = CIRCLE ( 'NONE', #907, 239.0000000000000000 ) ;
#9000 = CARTESIAN_POINT ( 'NONE',  ( -246.2769436248093200, 9.326692435635235867, 7.550684327875636370 ) ) ;
#9001 = DIRECTION ( 'NONE',  ( 0.5887335932212970357, 0.5538822189107471816, -0.5887335932212867107 ) ) ;
#9002 = CARTESIAN_POINT ( 'NONE',  ( -229.9414646403920699, -10.54384660290364728, 5.199876785550554992 ) ) ;
#9003 = PRODUCT_DEFINITION_SHAPE ( 'NONE', 'NONE',  #13115 ) ;
#9005 = EDGE_CURVE ( 'NONE', #5611, #2751, #6031, .T. ) ;
#9004 = CIRCLE ( 'NONE', #8581, 1.000000000000000000 ) ;
#9006 = EDGE_CURVE ( 'NONE', #4577, #889, #1009, .T. ) ;
#9007 = CARTESIAN_POINT ( 'NONE',  ( -229.9988845225136629, -11.97869403736654803, 0.7401432946465542617 ) ) ;
#9008 = EDGE_LOOP ( 'NONE', ( #6044, #10703 ) ) ;
#9009 = ORIENTED_EDGE ( 'NONE', *, *, #9934, .T. ) ;
#9010 = DIRECTION ( 'NONE',  ( 1.000000000000000000, 0.000000000000000000, 0.000000000000000000 ) ) ;
#9011 = DIRECTION ( 'NONE',  ( 0.000000000000000000, 1.000000000000000000, 0.000000000000000000 ) ) ;
#9012 = EDGE_CURVE ( 'NONE', #2751, #5611, #75, .T. ) ;
#9013 = CARTESIAN_POINT ( 'NONE',  ( 0.000000000000000000, -11.79660968244690089, 0.000000000000000000 ) ) ;
#9014 = AXIS2_PLACEMENT_3D ( 'NONE', #5378, #321, #124 ) ;
#9015 = CARTESIAN_POINT ( 'NONE',  ( 71.82423009839129691, 30.00000000000000000, -192.2354503650404922 ) ) ;
#9016 = DIRECTION ( 'NONE',  ( -0.9659258262890699775, 0.000000000000000000, 0.2588190451025145777 ) ) ;
#9017 = TOROIDAL_SURFACE ( 'NONE', #8177, 238.4705882352940307, 2.000000000000000000 ) ;
#9018 = DIRECTION ( 'NONE',  ( -0.000000000000000000, -1.000000000000000000, 0.000000000000000000 ) ) ;
#9019 = ITEM_DEFINED_TRANSFORMATION ( 'NONE', 'NONE', #2510,  #805 ) ;
#9020 = AXIS2_PLACEMENT_3D ( 'NONE', #12141, #4068, #5060 ) ;
#9021 = ORIENTED_EDGE ( 'NONE', *, *, #10342, .F. ) ;
#9022 = PLANE ( 'NONE',  #632 ) ;
#9023 = ADVANCED_FACE ( 'NONE', ( #9182 ), #2797, .T. ) ;
#9024 = DIRECTION ( 'NONE',  ( 0.6368676505102737195, 0.000000000000000000, 0.7709731485165509657 ) ) ;
#9025 = ORIENTED_EDGE ( 'NONE', *, *, #135, .T. ) ;
#9026 = ORIENTED_EDGE ( 'NONE', *, *, #1678, .T. ) ;
#9027 = CIRCLE ( 'NONE', #12008, 6.500000000000005329 ) ;
#9028 = CARTESIAN_POINT ( 'NONE',  ( -194.2446334056326123, 0.000000000000000000, -235.1468102975487682 ) ) ;
#9029 = EDGE_LOOP ( 'NONE', ( #4911, #2329 ) ) ;
#9030 = DIRECTION ( 'NONE',  ( -0.000000000000000000, -1.000000000000000000, 0.000000000000000000 ) ) ;
#9031 = CARTESIAN_POINT ( 'NONE',  ( -261.1558126970361400, 19.96883746064829168, 17.09264059829825300 ) ) ;
#9032 = FACE_OUTER_BOUND ( 'NONE', #7500, .T. ) ;
#9033 =( LENGTH_UNIT ( ) NAMED_UNIT ( * ) SI_UNIT ( .MILLI., .METRE. ) );
#9034 = CARTESIAN_POINT ( 'NONE',  ( -242.2132964870923502, 6.511711374314640643, 9.780601349828243585 ) ) ;
#9035 = ORIENTED_EDGE ( 'NONE', *, *, #117, .F. ) ;
#9036 = LINE ( 'NONE', #3829, #1144 ) ;
#9037 = ORIENTED_EDGE ( 'NONE', *, *, #763, .F. ) ;
#9038 = CARTESIAN_POINT ( 'NONE',  ( 165.7021400752469731, 1.848645179581459796, 200.5941117395221340 ) ) ;
#9039 = VERTEX_POINT ( 'NONE', #6950 ) ;
#9040 = CIRCLE ( 'NONE', #104, 5.500000000000015099 ) ;
#9041 = CARTESIAN_POINT ( 'NONE',  ( 0.000000000000000000, 22.00000000000000000, 0.000000000000000000 ) ) ;
#9042 = CARTESIAN_POINT ( 'NONE',  ( 122.2593324768334071, 19.00000000000000000, -162.7755348299894820 ) ) ;
#9043 = CARTESIAN_POINT ( 'NONE',  ( 0.000000000000000000, 0.000000000000000000, 0.000000000000000000 ) ) ;
#9044 = LINE ( 'NONE', #5098, #11551 ) ;
#9045 = CARTESIAN_POINT ( 'NONE',  ( 71.82423009839129691, 19.40000000000000213, -192.2354503650404922 ) ) ;
#9046 = CARTESIAN_POINT ( 'NONE',  ( -241.4851975124299486, -5.604998872266711452, 10.61066964827916337 ) ) ;
#9047 = CARTESIAN_POINT ( 'NONE',  ( -238.8209209945083273, 0.7687232794247820244, -11.97535954144907500 ) ) ;
#9048 = CONTEXT_DEPENDENT_SHAPE_REPRESENTATION ( #8226, #3291 ) ;
#9049 = EDGE_LOOP ( 'NONE', ( #4165, #5689, #9884, #1562, #3255, #6242, #10093, #12936, #6877, #5924, #11431, #1776 ) ) ;
#9050 = CYLINDRICAL_SURFACE ( 'NONE', #11316, 250.1999999999999602 ) ;
#9051 =( GEOMETRIC_REPRESENTATION_CONTEXT ( 3 ) GLOBAL_UNCERTAINTY_ASSIGNED_CONTEXT ( ( #5987 ) ) GLOBAL_UNIT_ASSIGNED_CONTEXT ( ( #867, #12005, #9066 ) ) REPRESENTATION_CONTEXT ( 'NONE', 'WORKASPACE' ) );
#9052 = ORIENTED_EDGE ( 'NONE', *, *, #8587, .F. ) ;
#9053 = ADVANCED_FACE ( 'NONE', ( #4874 ), #8150, .F. ) ;
#9054 = EDGE_CURVE ( 'NONE', #6584, #9162, #8950, .T. ) ;
#9055 = ORIENTED_EDGE ( 'NONE', *, *, #253, .F. ) ;
#9056 = DIRECTION ( 'NONE',  ( -0.000000000000000000, -1.000000000000000000, 0.000000000000000000 ) ) ;
#9057 = EDGE_LOOP ( 'NONE', ( #13028, #9777, #9451 ) ) ;
#9058 = CARTESIAN_POINT ( 'NONE',  ( 226.7975291061089820, 20.55460285063310621, -130.9697226050975019 ) ) ;
#9059 = FACE_OUTER_BOUND ( 'NONE', #6986, .T. ) ;
#9060 = CARTESIAN_POINT ( 'NONE',  ( 227.3999999999999773, 0.000000000000000000, 0.000000000000000000 ) ) ;
#9061 = DIRECTION ( 'NONE',  ( 0.000000000000000000, -1.000000000000000000, 0.000000000000000000 ) ) ;
#9062 = CONICAL_SURFACE ( 'NONE', #9913, 6.500000000000026645, 0.7853981633974476129 ) ;
#9063 = VECTOR ( 'NONE', #12434, 1000.000000000000114 ) ;
#9064 = CARTESIAN_POINT ( 'NONE',  ( -242.6194444007928439, 6.961689675959383372, 9.776526357768153375 ) ) ;
#9065 = PRODUCT_DEFINITION ( 'UNKNOWN', '', #10872, #9950 ) ;
#9066 =( NAMED_UNIT ( * ) SI_UNIT ( $, .STERADIAN. ) SOLID_ANGLE_UNIT ( ) );
#9067 = DIRECTION ( 'NONE',  ( 0.2588190451025314531, 0.000000000000000000, -0.9659258262890654256 ) ) ;
#9068 = LINE ( 'NONE', #4925, #7763 ) ;
#9069 = ITEM_DEFINED_TRANSFORMATION ( 'NONE', 'NONE', #10859,  #805 ) ;
#9070 = DIRECTION ( 'NONE',  ( 0.000000000000000000, 0.000000000000000000, -1.000000000000000000 ) ) ;
#9071 = ORIENTED_EDGE ( 'NONE', *, *, #12357, .T. ) ;
#9072 = EDGE_LOOP ( 'NONE', ( #10067, #1367, #9948, #6204 ) ) ;
#9073 = CARTESIAN_POINT ( 'NONE',  ( 5.000000000000000000, 9.797174393178815797E-16, 242.0000000000000000 ) ) ;
#9074 = DIRECTION ( 'NONE',  ( 0.000000000000000000, 0.000000000000000000, 1.000000000000000000 ) ) ;
#9075 = FACE_OUTER_BOUND ( 'NONE', #1301, .T. ) ;
#9076 = ADVANCED_FACE ( 'NONE', ( #1818 ), #2820, .F. ) ;
#9077 = DIRECTION ( 'NONE',  ( 0.000000000000000000, 0.000000000000000000, 1.000000000000000000 ) ) ;
#9078 = ADVANCED_FACE ( 'NONE', ( #12018 ), #5886, .F. ) ;
#9079 = FACE_OUTER_BOUND ( 'NONE', #12748, .T. ) ;
#9080 = DIRECTION ( 'NONE',  ( 0.7660444431189706860, 0.000000000000000000, 0.6427876096865481337 ) ) ;
#9081 = CARTESIAN_POINT ( 'NONE',  ( 225.1241593668336236, -30.00000000000000000, -185.9653539489990521 ) ) ;
#9082 = CONTEXT_DEPENDENT_SHAPE_REPRESENTATION ( #299, #7234 ) ;
#9083 = ORIENTED_EDGE ( 'NONE', *, *, #5837, .F. ) ;
#9084 =( REPRESENTATION_RELATIONSHIP ('NONE','NONE', #12019, #182 ) REPRESENTATION_RELATIONSHIP_WITH_TRANSFORMATION ( #11209 )SHAPE_REPRESENTATION_RELATIONSHIP( ) );
#9085 = CARTESIAN_POINT ( 'NONE',  ( 197.8197553893920144, 19.00000000000000000, 64.27553482998850143 ) ) ;
#9086 = CARTESIAN_POINT ( 'NONE',  ( -239.5355863986199836, -1.859542203694944051, 11.85503690034565416 ) ) ;
#9087 = ORIENTED_EDGE ( 'NONE', *, *, #7292, .F. ) ;
#9088 = ORIENTED_EDGE ( 'NONE', *, *, #2012, .T. ) ;
#9089 = DIRECTION ( 'NONE',  ( 0.000000000000000000, 1.000000000000000000, 0.000000000000000000 ) ) ;
#9090 = CARTESIAN_POINT ( 'NONE',  ( 0.000000000000000000, 0.000000000000000000, 0.000000000000000000 ) ) ;
#9091 = CARTESIAN_POINT ( 'NONE',  ( -249.6759349623767434, 11.17873215479417581, 3.619182054004953741 ) ) ;
#9092 = CARTESIAN_POINT ( 'NONE',  ( 226.1171533156415023, 20.08915143315739726, 130.5770120865019805 ) ) ;
#9093 = ADVANCED_FACE ( 'NONE', ( #3941 ), #18, .F. ) ;
#9094 = CARTESIAN_POINT ( 'NONE',  ( -238.9264504976112846, -1.042958814602677364, -11.95497062546909639 ) ) ;
#9095 =( NAMED_UNIT ( * ) SI_UNIT ( $, .STERADIAN. ) SOLID_ANGLE_UNIT ( ) );
#9096 = CARTESIAN_POINT ( 'NONE',  ( -243.2136795380932313, 7.496740017165948622, 9.047741631695624065 ) ) ;
#9097 = ORIENTED_EDGE ( 'NONE', *, *, #6973, .F. ) ;
#9098 = CARTESIAN_POINT ( 'NONE',  ( 287.1814104624967854, -19.00000000000000000, 23.44910453727082356 ) ) ;
#9099 = ORIENTED_EDGE ( 'NONE', *, *, #5467, .F. ) ;
#9100 = CARTESIAN_POINT ( 'NONE',  ( -245.3969493176502397, 8.938055201219498258, -7.627167029064186643 ) ) ;
#9101 = EDGE_LOOP ( 'NONE', ( #7651, #9680, #11503, #417 ) ) ;
#9102 = CIRCLE ( 'NONE', #1866, 5.500000000000015099 ) ;
#9103 = CARTESIAN_POINT ( 'NONE',  ( 122.2593324768346008, 30.00000000000000000, 168.2755348299889988 ) ) ;
#9104 = DIRECTION ( 'NONE',  ( -0.000000000000000000, -1.000000000000000000, 0.000000000000000000 ) ) ;
#9105 = DIRECTION ( 'NONE',  ( 1.000000000000000000, 0.000000000000000000, 0.000000000000000000 ) ) ;
#9106 = CARTESIAN_POINT ( 'NONE',  ( -59.19439222780410148, 20.08915143297736705, -253.8843055347119275 ) ) ;
#9107 = PRODUCT_DEFINITION_SHAPE ( 'NONE', 'NONE',  #13141 ) ;
#9108 = LINE ( 'NONE', #11110, #704 ) ;
#9109 = AXIS2_PLACEMENT_3D ( 'NONE', #12429, #5149, #1093 ) ;
#9110 = CARTESIAN_POINT ( 'NONE',  ( -238.7910754938288846, 0.6701662195168923697, -11.98127733922759042 ) ) ;
#9111 = VERTEX_POINT ( 'NONE', #86 ) ;
#9112 = FACE_OUTER_BOUND ( 'NONE', #9188, .T. ) ;
#9113 = ORIENTED_EDGE ( 'NONE', *, *, #11373, .F. ) ;
#9114 = CARTESIAN_POINT ( 'NONE',  ( -247.8064210917818855, -9.777989738504603068, -6.956369377821547850 ) ) ;
#9115 = CARTESIAN_POINT ( 'NONE',  ( -249.3105109839375189, -10.55009524026396228, 5.172972615363025106 ) ) ;
#9116 = VERTEX_POINT ( 'NONE', #12074 ) ;
#9117 = AXIS2_PLACEMENT_3D ( 'NONE', #5352, #9356, #5145 ) ;
#9118 = AXIS2_PLACEMENT_3D ( 'NONE', #9345, #8352, #212 ) ;
#9119 = CARTESIAN_POINT ( 'NONE',  ( 115.5625104412701916, 20.79694577657783228, 234.3927740975209986 ) ) ;
#9120 = CARTESIAN_POINT ( 'NONE',  ( -246.6520855319178906, 9.461709547860877478, -7.381047754363233793 ) ) ;
#9121 = FACE_OUTER_BOUND ( 'NONE', #3089, .T. ) ;
#9122 = CARTESIAN_POINT ( 'NONE',  ( -244.4357566112991549, -8.400224617168833063, -8.216123742228331750 ) ) ;
#9123 = EDGE_CURVE ( 'NONE', #9288, #5992, #9854, .T. ) ;
#9124 = CARTESIAN_POINT ( 'NONE',  ( -244.7098307144296996, 8.574293600822041839, 8.395350236016119183 ) ) ;
#9125 = EDGE_CURVE ( 'NONE', #10768, #9111, #8081, .T. ) ;
#9126 = SURFACE_STYLE_FILL_AREA ( #7929 ) ;
#9127 = DIRECTION ( 'NONE',  ( 0.8294267566935203950, 0.5538822189107471816, 0.07256543843576650221 ) ) ;
#9128 = CARTESIAN_POINT ( 'NONE',  ( -229.8105890609549817, -7.167558729527323536, 9.342082834280224901 ) ) ;
#9129 = ITEM_DEFINED_TRANSFORMATION ( 'NONE', 'NONE', #3192,  #805 ) ;
#9130 = VECTOR ( 'NONE', #1660, 1000.000000000000114 ) ;
#9131 = CIRCLE ( 'NONE', #1461, 6.500000000000005329 ) ;
#9132 = AXIS2_PLACEMENT_3D ( 'NONE', #2739, #9089, #3420 ) ;
#9133 = DIRECTION ( 'NONE',  ( 0.6368676505102700558, 0.000000000000000000, 0.7709731485165541853 ) ) ;
#9134 = VERTEX_POINT ( 'NONE', #8015 ) ;
#9135 = EDGE_LOOP ( 'NONE', ( #10210, #1297, #5430, #8128 ) ) ;
#9136 = CARTESIAN_POINT ( 'NONE',  ( 234.1947771726669885, 20.08915143309429041, 115.4648407708036046 ) ) ;
#9137 = CARTESIAN_POINT ( 'NONE',  ( 197.8197553893920144, 30.00000000000000000, 57.77553482998850143 ) ) ;
#9138 = DIRECTION ( 'NONE',  ( 0.000000000000000000, -1.000000000000000000, 0.000000000000000000 ) ) ;
#9139 = CIRCLE ( 'NONE', #1900, 6.500000000000005329 ) ;
#9140 = DIRECTION ( 'NONE',  ( 0.000000000000000000, 0.000000000000000000, 1.000000000000000000 ) ) ;
#9141 = DIRECTION ( 'NONE',  ( 0.6368676505102707219, 0.000000000000000000, 0.7709731485165535192 ) ) ;
#9142 = AXIS2_PLACEMENT_3D ( 'NONE', #12080, #1823, #1015 ) ;
#9143 = DIRECTION ( 'NONE',  ( 1.047444401652940007E-14, 0.000000000000000000, -1.000000000000000000 ) ) ;
#9144 = CARTESIAN_POINT ( 'NONE',  ( -241.5622318746700046, -5.708434620867652853, 10.27645530603111723 ) ) ;
#9145 =( REPRESENTATION_RELATIONSHIP ('NONE','NONE', #12019, #182 ) REPRESENTATION_RELATIONSHIP_WITH_TRANSFORMATION ( #10368 )SHAPE_REPRESENTATION_RELATIONSHIP( ) );
#9146 = VERTEX_POINT ( 'NONE', #6148 ) ;
#9147 = DIRECTION ( 'NONE',  ( 0.000000000000000000, 1.000000000000000000, 0.000000000000000000 ) ) ;
#9148 = AXIS2_PLACEMENT_3D ( 'NONE', #7400, #10133, #9276 ) ;
#9149 = CARTESIAN_POINT ( 'NONE',  ( 229.9733680233431130, -0.2284314955805349379, -3.499999999999966249 ) ) ;
#9150 = EDGE_LOOP ( 'NONE', ( #5312, #1638, #3035, #2956 ) ) ;
#9151 = ORIENTED_EDGE ( 'NONE', *, *, #1586, .T. ) ;
#9152 = EDGE_CURVE ( 'NONE', #2361, #10957, #3874, .T. ) ;
#9153 = AXIS2_PLACEMENT_3D ( 'NONE', #256, #12582, #6523 ) ;
#9154 = EDGE_CURVE ( 'NONE', #12564, #8176, #4073, .T. ) ;
#9155 = CARTESIAN_POINT ( 'NONE',  ( 0.000000000000000000, -22.00000000000000000, 0.000000000000000000 ) ) ;
#9156 = DIRECTION ( 'NONE',  ( 0.000000000000000000, 0.7071067811865480168, 0.7071067811865470176 ) ) ;
#9157 = CARTESIAN_POINT ( 'NONE',  ( -84.14846197923118609, 19.96883746246331981, 247.8175805181506348 ) ) ;
#9158 = CARTESIAN_POINT ( 'NONE',  ( -239.4322611284946731, -1.761824011993069705, -11.86996097360714053 ) ) ;
#9159 = DIRECTION ( 'NONE',  ( 0.9848077530122080203, 0.000000000000000000, 0.1736481776669307198 ) ) ;
#9160 = CARTESIAN_POINT ( 'NONE',  ( -245.0777337327412795, 8.776737542119800395, 7.814324100309848475 ) ) ;
#9161 = AXIS2_PLACEMENT_3D ( 'NONE', #10322, #7264, #7192 ) ;
#9162 = VERTEX_POINT ( 'NONE', #1945 ) ;
#9163 = DIRECTION ( 'NONE',  ( 0.6368676505102716101, 0.000000000000000000, 0.7709731485165527420 ) ) ;
#9164 = ORIENTED_EDGE ( 'NONE', *, *, #8186, .F. ) ;
#9165 = AXIS2_PLACEMENT_3D ( 'NONE', #4399, #1413, #12417 ) ;
#9166 = DIRECTION ( 'NONE',  ( 0.000000000000000000, 0.9998057603070480415, -0.01970892327970899874 ) ) ;
#9167 = ORIENTED_EDGE ( 'NONE', *, *, #10184, .T. ) ;
#9168 = ADVANCED_FACE ( 'NONE', ( #5005 ), #7521, .F. ) ;
#9169 = CARTESIAN_POINT ( 'NONE',  ( 0.000000000000000000, -20.69999999999999929, 0.000000000000000000 ) ) ;
#9170 = PRODUCT_DEFINITION_FORMATION_WITH_SPECIFIED_SOURCE ( 'ANY', '', #334, .NOT_KNOWN. ) ;
#9171 = DIRECTION ( 'NONE',  ( 0.000000000000000000, 1.000000000000000000, 0.000000000000000000 ) ) ;
#9172 = LINE ( 'NONE', #6108, #419 ) ;
#9173 = CARTESIAN_POINT ( 'NONE',  ( 122.2593324768334071, 19.00000000000000000, -168.2755348299895104 ) ) ;
#9174 = ADVANCED_FACE ( 'NONE', ( #9079 ), #1075, .F. ) ;
#9175 = CARTESIAN_POINT ( 'NONE',  ( -285.6731895343928613, -30.00000000000000000, 15.42881051422395622 ) ) ;
#9176 = CARTESIAN_POINT ( 'NONE',  ( -159.2169126275676945, -3.061616997868385015E-14, -192.7432871291383663 ) ) ;
#9177 = PLANE ( 'NONE',  #2659 ) ;
#9178 = ITEM_DEFINED_TRANSFORMATION ( 'NONE', 'NONE', #8285,  #805 ) ;
#9179 = ORIENTED_EDGE ( 'NONE', *, *, #9803, .F. ) ;
#9180 = CARTESIAN_POINT ( 'NONE',  ( 0.000000000000000000, 29.00000000000000000, 0.000000000000000000 ) ) ;
#9181 = TOROIDAL_SURFACE ( 'NONE', #884, 250.0000000000000000, 10.00000000000000000 ) ;
#9182 = FACE_OUTER_BOUND ( 'NONE', #2440, .T. ) ;
#9183 = EDGE_LOOP ( 'NONE', ( #12355, #2520, #2004, #12051 ) ) ;
#9184 = AXIS2_PLACEMENT_3D ( 'NONE', #7577, #6387, #12512 ) ;
#9185 = CARTESIAN_POINT ( 'NONE',  ( -249.2062170167872068, 10.43176588139601257, -5.409795435560969423 ) ) ;
#9186 = CARTESIAN_POINT ( 'NONE',  ( -244.6090102803748607, -8.514624250321579879, -8.455955372765057376 ) ) ;
#9187 = DIRECTION ( 'NONE',  ( 0.000000000000000000, -1.000000000000000000, 0.000000000000000000 ) ) ;
#9188 = EDGE_LOOP ( 'NONE', ( #5755, #1722, #10547, #4640 ) ) ;
#9189 = VECTOR ( 'NONE', #7041, 1000.000000000000000 ) ;
#9190 = CARTESIAN_POINT ( 'NONE',  ( -115.5625104412419972, 20.79694577648909615, -234.3927740977559893 ) ) ;
#9191 = CARTESIAN_POINT ( 'NONE',  ( -249.3376476198023681, 9.985526825732678802, -6.655116011130676412 ) ) ;
#9192 = CARTESIAN_POINT ( 'NONE',  ( 229.9000000000000057, -0.1024105694488001289, -5.195143123655522110 ) ) ;
#9193 = CARTESIAN_POINT ( 'NONE',  ( -243.2454781611184274, -7.524012747006318946, -9.025130280554842344 ) ) ;
#9194 = CARTESIAN_POINT ( 'NONE',  ( 172.3268284095375122, 20.79694577629726027, -196.4640694357605071 ) ) ;
#9195 = DIRECTION ( 'NONE',  ( -0.5735764363510391650, 0.000000000000000000, -0.8191520442889966835 ) ) ;
#9196 = FACE_OUTER_BOUND ( 'NONE', #10722, .T. ) ;
#9197 = ITEM_DEFINED_TRANSFORMATION ( 'NONE', 'NONE', #4468,  #805 ) ;
#9198 = LINE ( 'NONE', #12400, #7077 ) ;
#9199 = ORIENTED_EDGE ( 'NONE', *, *, #6741, .T. ) ;
#9200 = EDGE_LOOP ( 'NONE', ( #3298, #11780, #5158, #12731 ) ) ;
#9201 = AXIS2_PLACEMENT_3D ( 'NONE', #4235, #1179, #8317 ) ;
#9202 = EDGE_CURVE ( 'NONE', #2804, #320, #10135, .T. ) ;
#9203 = CARTESIAN_POINT ( 'NONE',  ( 226.1171533175249806, 20.08915143274010262, -130.5770120874387885 ) ) ;
#9204 = CARTESIAN_POINT ( 'NONE',  ( 234.4000000000000057, 0.000000000000000000, 0.000000000000000000 ) ) ;
#9205 = VECTOR ( 'NONE', #149, 1000.000000000000000 ) ;
#9206 = DIRECTION ( 'NONE',  ( -0.000000000000000000, -1.000000000000000000, 0.000000000000000000 ) ) ;
#9207 = CARTESIAN_POINT ( 'NONE',  ( 0.000000000000000000, 19.00000000000000000, 0.000000000000000000 ) ) ;
#9208 = CARTESIAN_POINT ( 'NONE',  ( 196.4640694355999813, 20.79694577639575570, -172.3268284093740021 ) ) ;
#9209 = DIRECTION ( 'NONE',  ( 1.000000000000000000, 0.000000000000000000, 0.000000000000000000 ) ) ;
#9210 = DIRECTION ( 'NONE',  ( 0.8660254037844450359, 0.000000000000000000, -0.4999999999999888978 ) ) ;
#9211 = AXIS2_PLACEMENT_3D ( 'NONE', #5838, #10218, #897 ) ;
#9212 = CARTESIAN_POINT ( 'NONE',  ( -243.1473425731909117, -7.439266815360506158, 9.095043743685003790 ) ) ;
#9213 = EDGE_LOOP ( 'NONE', ( #9947, #5626 ) ) ;
#9214 = CIRCLE ( 'NONE', #10707, 270.0000000000000000 ) ;
#9215 = CARTESIAN_POINT ( 'NONE',  ( 71.82423009839129691, 28.60000000000000142, -197.3354503650404865 ) ) ;
#9216 = FACE_OUTER_BOUND ( 'NONE', #3562, .T. ) ;
#9217 = ORIENTED_EDGE ( 'NONE', *, *, #12761, .T. ) ;
#9218 = EDGE_CURVE ( 'NONE', #6838, #8770, #12534, .T. ) ;
#9219 = ORIENTED_EDGE ( 'NONE', *, *, #12471, .F. ) ;
#9220 = EDGE_CURVE ( 'NONE', #8160, #6601, #6670, .T. ) ;
#9221 = CARTESIAN_POINT ( 'NONE',  ( 220.3999999999999773, 0.000000000000000000, 0.000000000000000000 ) ) ;
#9222 = CARTESIAN_POINT ( 'NONE',  ( 0.000000000000000000, 24.99999999999995737, -250.3823410207189966 ) ) ;
#9223 = PRODUCT_DEFINITION_SHAPE ( 'NONE', 'NONE',  #13129 ) ;
#9224 = TOROIDAL_SURFACE ( 'NONE', #4316, 6.053020646647509828, 3.153020646647509917 ) ;
#9225 = AXIS2_PLACEMENT_3D ( 'NONE', #7493, #8560, #9607 ) ;
#9226 = CLOSED_SHELL ( 'NONE', ( #12705, #11106, #1060, #6746, #9980, #4652, #848, #5567, #5512, #5238 ) ) ;
#9227 = CARTESIAN_POINT ( 'NONE',  ( 67.71318189755788808, 19.96883746081500988, -252.8031682274115894 ) ) ;
#9228 = CARTESIAN_POINT ( 'NONE',  ( -238.7907910596442207, -0.6691544179571565776, -11.98133399144852440 ) ) ;
#9229 = CIRCLE ( 'NONE', #508, 239.0000000000000000 ) ;
#9230 = DIRECTION ( 'NONE',  ( 0.000000000000000000, 0.000000000000000000, 1.000000000000000000 ) ) ;
#9231 = CARTESIAN_POINT ( 'NONE',  ( -245.5121636011789690, 8.994012744481606703, 7.561165849620649304 ) ) ;
#9232 = ADVANCED_FACE ( 'NONE', ( #6285 ), #10539, .F. ) ;
#9233 = ORIENTED_EDGE ( 'NONE', *, *, #12084, .F. ) ;
#9234 = CARTESIAN_POINT ( 'NONE',  ( 225.1241593668336236, -18.00000000000000000, -185.9653539489990521 ) ) ;
#9235 = AXIS2_PLACEMENT_3D ( 'NONE', #2768, #10047, #6856 ) ;
#9236 = ORIENTED_EDGE ( 'NONE', *, *, #10581, .T. ) ;
#9237 = CONICAL_SURFACE ( 'NONE', #3477, 5.500000000000015099, 0.7853981633974461696 ) ;
#9238 = EDGE_LOOP ( 'NONE', ( #10005, #3168 ) ) ;
#9239 = CYLINDRICAL_SURFACE ( 'NONE', #5996, 5.100000000000003197 ) ;
#9240 = SURFACE_STYLE_FILL_AREA ( #2169 ) ;
#9241 = CARTESIAN_POINT ( 'NONE',  ( 239.1910253111598479, 1.013189013438377417, 3.350157823592870177 ) ) ;
#9242 = FACE_OUTER_BOUND ( 'NONE', #4207, .T. ) ;
#9243 = DIRECTION ( 'NONE',  ( 0.6368676505102708330, 0.000000000000000000, 0.7709731485165535192 ) ) ;
#9244 = CARTESIAN_POINT ( 'NONE',  ( 0.000000000000000000, 19.00000000000000000, 0.000000000000000000 ) ) ;
#9245 = EDGE_CURVE ( 'NONE', #9508, #3688, #1775, .T. ) ;
#9246 = ADVANCED_FACE ( 'NONE', ( #9528 ), #12382, .F. ) ;
#9247 = CARTESIAN_POINT ( 'NONE',  ( -190.4297758776781393, 20.79694577634646180, 178.3611219674581037 ) ) ;
#9248 = CONTEXT_DEPENDENT_SHAPE_REPRESENTATION ( #5231, #4256 ) ;
#9249 = VERTEX_POINT ( 'NONE', #10335 ) ;
#9250 = VECTOR ( 'NONE', #10840, 1000.000000000000000 ) ;
#9251 = DIRECTION ( 'NONE',  ( 0.000000000000000000, 0.000000000000000000, -1.000000000000000000 ) ) ;
#9252 = ORIENTED_EDGE ( 'NONE', *, *, #12273, .T. ) ;
#9253 = DIRECTION ( 'NONE',  ( 0.000000000000000000, 1.000000000000000000, 0.000000000000000000 ) ) ;
#9254 = CARTESIAN_POINT ( 'NONE',  ( -247.3711767290720616, -9.676486748149162764, -7.096931843143912566 ) ) ;
#9255 = VECTOR ( 'NONE', #771, 1000.000000000000000 ) ;
#9256 = CIRCLE ( 'NONE', #4558, 6.500000000000000888 ) ;
#9257 = CARTESIAN_POINT ( 'NONE',  ( -249.2062170165277166, -10.43176588117700021, 5.409795435997606816 ) ) ;
#9258 = ORIENTED_EDGE ( 'NONE', *, *, #1419, .T. ) ;
#9259 = CARTESIAN_POINT ( 'NONE',  ( -34.13493237021134519, 20.79694577641179620, -259.0935598599534728 ) ) ;
#9260 = CARTESIAN_POINT ( 'NONE',  ( -240.5954930647663161, 4.058997395297933686, -11.29299565157840668 ) ) ;
#9261 = DIRECTION ( 'NONE',  ( 0.000000000000000000, 0.9998057603070481525, -0.01970892327970899874 ) ) ;
#9262 =( REPRESENTATION_RELATIONSHIP ('NONE','NONE', #12019, #5191 ) REPRESENTATION_RELATIONSHIP_WITH_TRANSFORMATION ( #11868 )SHAPE_REPRESENTATION_RELATIONSHIP( ) );
#9263 = CARTESIAN_POINT ( 'NONE',  ( -243.4706526255369283, -7.711678295906986058, -8.866250711340882162 ) ) ;
#9264 = VECTOR ( 'NONE', #1746, 1000.000000000000000 ) ;
#9265 = EDGE_CURVE ( 'NONE', #564, #2972, #7936, .T. ) ;
#9266 = PRODUCT_DEFINITION_SHAPE ( 'NONE', 'NONE',  #13047 ) ;
#9267 = DIRECTION ( 'NONE',  ( 0.6820219226572490356, 0.5538822189107470706, -0.4775568914688768096 ) ) ;
#9268 = DIRECTION ( 'NONE',  ( -0.6368676505102698338, 0.000000000000000000, -0.7709731485165541853 ) ) ;
#9269 = CARTESIAN_POINT ( 'NONE',  ( 122.2593324768346008, 30.00000000000000000, 168.2755348299889988 ) ) ;
#9270 = ORIENTED_EDGE ( 'NONE', *, *, #6294, .F. ) ;
#9271 = ORIENTED_EDGE ( 'NONE', *, *, #12346, .F. ) ;
#9272 = COLOUR_RGB ( '', 0.08235294, 0.09019608, 0.10196078) ;
#9273 = CARTESIAN_POINT ( 'NONE',  ( -172.1812796675209825, 20.08915143307664053, -196.2980642830465001 ) ) ;
#9274 = DIRECTION ( 'NONE',  ( 0.000000000000000000, -1.000000000000000000, 0.000000000000000000 ) ) ;
#9275 = AXIS2_PLACEMENT_3D ( 'NONE', #12369, #5157, #8309 ) ;
#9276 = DIRECTION ( 'NONE',  ( 0.000000000000000000, 0.9998057603070481525, -0.01970892327970900221 ) ) ;
#9277 = LINE ( 'NONE', #11470, #4758 ) ;
#9278 = LINE ( 'NONE', #11723, #9205 ) ;
#9279 = DIRECTION ( 'NONE',  ( 0.000000000000000000, 0.000000000000000000, -1.000000000000000000 ) ) ;
#9280 = DIRECTION ( 'NONE',  ( 0.9063077870366553768, 0.000000000000000000, -0.4226182617406879505 ) ) ;
#9281 = FACE_OUTER_BOUND ( 'NONE', #8142, .T. ) ;
#9282 = AXIS2_PLACEMENT_3D ( 'NONE', #11597, #8716, #12651 ) ;
#9283 = ORIENTED_EDGE ( 'NONE', *, *, #9825, .F. ) ;
#9284 = CARTESIAN_POINT ( 'NONE',  ( 240.3826708216964789, -2.772967769359314882, -2.135567781667015108 ) ) ;
#9285 = CIRCLE ( 'NONE', #10985, 6.500000000000005329 ) ;
#9286 = CARTESIAN_POINT ( 'NONE',  ( 229.9983178831911630, -3.387952982252648404, -0.9078284637049901518 ) ) ;
#9287 = ORIENTED_EDGE ( 'NONE', *, *, #9904, .T. ) ;
#9288 = VERTEX_POINT ( 'NONE', #2139 ) ;
#9289 = CARTESIAN_POINT ( 'NONE',  ( 240.3371538976037982, -2.621326596188751079, 2.332469087876801517 ) ) ;
#9290 = CARTESIAN_POINT ( 'NONE',  ( -293.9524689910264215, -30.00000000000000000, 5.406159583508762800 ) ) ;
#9291 = CARTESIAN_POINT ( 'NONE',  ( 234.1947771728840166, 20.08915143305504714, -115.4648407707930033 ) ) ;
#9292 = DIRECTION ( 'NONE',  ( 0.000000000000000000, 0.000000000000000000, -1.000000000000000000 ) ) ;
#9293 = CARTESIAN_POINT ( 'NONE',  ( 0.000000000000000000, 0.000000000000000000, 0.000000000000000000 ) ) ;
#9294 = CARTESIAN_POINT ( 'NONE',  ( -245.4374131353386304, 8.957880035620332748, 7.603877364227019875 ) ) ;
#9295 = ADVANCED_FACE ( 'NONE', ( #11412 ), #12833, .F. ) ;
#9296 = ADVANCED_FACE ( 'NONE', ( #408 ), #3888, .F. ) ;
#9297 = ORIENTED_EDGE ( 'NONE', *, *, #7951, .T. ) ;
#9298 = LINE ( 'NONE', #12238, #8394 ) ;
#9299 = ORIENTED_EDGE ( 'NONE', *, *, #11615, .F. ) ;
#9300 = DIRECTION ( 'NONE',  ( 0.000000000000000000, 0.000000000000000000, 1.000000000000000000 ) ) ;
#9301 = ORIENTED_EDGE ( 'NONE', *, *, #2955, .F. ) ;
#9302 = ORIENTED_EDGE ( 'NONE', *, *, #11298, .F. ) ;
#9303 = ADVANCED_FACE ( 'NONE', ( #5469 ), #3392, .F. ) ;
#9304 = CARTESIAN_POINT ( 'NONE',  ( 0.000000000000000000, -20.00000000000000000, 248.7999999999999829 ) ) ;
#9305 = DIRECTION ( 'NONE',  ( 1.000000000000000000, 0.000000000000000000, 0.000000000000000000 ) ) ;
#9306 = CARTESIAN_POINT ( 'NONE',  ( -0.000000000000000000, -18.00000000000000000, 0.000000000000000000 ) ) ;
#9307 = DIRECTION ( 'NONE',  ( 0.000000000000000000, 0.000000000000000000, -1.000000000000000000 ) ) ;
#9308 = CARTESIAN_POINT ( 'NONE',  ( -178.2104428091925854, 20.08915143297736350, -190.2689011420772260 ) ) ;
#9309 = AXIS2_PLACEMENT_3D ( 'NONE', #1418, #7551, #2412 ) ;
#9310 = FILL_AREA_STYLE_COLOUR ( '', #3247 ) ;
#9311 = ORIENTED_EDGE ( 'NONE', *, *, #4481, .T. ) ;
#9312 = DIRECTION ( 'NONE',  ( 0.6368676505102707219, 0.000000000000000000, 0.7709731485165535192 ) ) ;
#9314 = ORIENTED_EDGE ( 'NONE', *, *, #9890, .F. ) ;
#9313 = AXIS2_PLACEMENT_3D ( 'NONE', #4442, #10522, #8526 ) ;
#9315 = LINE ( 'NONE', #4244, #7632 ) ;
#9316 = CARTESIAN_POINT ( 'NONE',  ( -197.8197553893924976, 29.00000000000000000, -64.27553482998719403 ) ) ;
#9317 = CARTESIAN_POINT ( 'NONE',  ( -248.8927262316770737, -10.16869272925975309, 5.887412070189221858 ) ) ;
#9318 = VERTEX_POINT ( 'NONE', #12279 ) ;
#9319 = EDGE_CURVE ( 'NONE', #2094, #7035, #1342, .T. ) ;
#9320 = CARTESIAN_POINT ( 'NONE',  ( 260.7745447061710138, 20.79694577634646180, 17.06760680878259961 ) ) ;
#9321 = ADVANCED_FACE ( 'NONE', ( #9344 ), #5592, .F. ) ;
#9322 = CARTESIAN_POINT ( 'NONE',  ( -241.3090253319704743, 5.344653766046771004, -10.74405649903250470 ) ) ;
#9323 = CARTESIAN_POINT ( 'NONE',  ( 0.000000000000000000, 29.00000000000000000, -208.0000000000000000 ) ) ;
#9324 = CARTESIAN_POINT ( 'NONE',  ( -247.3797639054675415, -9.674571922432775750, -6.668012154483388798 ) ) ;
#9325 = AXIS2_PLACEMENT_3D ( 'NONE', #898, #12362, #3215 ) ;
#9326 = APPLICATION_CONTEXT ( 'automotive_design' ) ;
#9327 =( NAMED_UNIT ( * ) PLANE_ANGLE_UNIT ( ) SI_UNIT ( $, .RADIAN. ) );
#9328 = CARTESIAN_POINT ( 'NONE',  ( 29.59329699131349045, -138.4705547276867321, 29.59329699131421165 ) ) ;
#9329 = DIRECTION ( 'NONE',  ( 0.6368676505102716101, 0.000000000000000000, 0.7709731485165527420 ) ) ;
#9330 = CONTEXT_DEPENDENT_SHAPE_REPRESENTATION ( #3822, #5915 ) ;
#9331 = AXIS2_PLACEMENT_3D ( 'NONE', #4876, #1752, #9016 ) ;
#9332 = FACE_OUTER_BOUND ( 'NONE', #7880, .T. ) ;
#9333 = ORIENTED_EDGE ( 'NONE', *, *, #5016, .F. ) ;
#9334 = CARTESIAN_POINT ( 'NONE',  ( -1.008906662707803564E-12, 19.96883746059272724, 261.1558126970361400 ) ) ;
#9335 = ADVANCED_FACE ( 'NONE', ( #1145 ), #11474, .T. ) ;
#9336 = CARTESIAN_POINT ( 'NONE',  ( 159.3442861576696998, -21.50000000000000000, 192.8974817588416784 ) ) ;
#9337 =( REPRESENTATION_RELATIONSHIP ('NONE','NONE', #12019, #182 ) REPRESENTATION_RELATIONSHIP_WITH_TRANSFORMATION ( #2073 )SHAPE_REPRESENTATION_RELATIONSHIP( ) );
#9338 = CARTESIAN_POINT ( 'NONE',  ( 197.8197553893920144, 30.00000000000000000, 70.77553482998851564 ) ) ;
#9339 = DIRECTION ( 'NONE',  ( 0.000000000000000000, -1.000000000000000000, 0.000000000000000000 ) ) ;
#9340 = AXIS2_PLACEMENT_3D ( 'NONE', #1626, #9745, #3889 ) ;
#9341 = CARTESIAN_POINT ( 'NONE',  ( -247.6787047799290065, -9.753293421073170322, 6.991498263521549461 ) ) ;
#9342 = EDGE_CURVE ( 'NONE', #11150, #9966, #12204, .T. ) ;
#9343 = CIRCLE ( 'NONE', #11689, 8.000000000000007105 ) ;
#9344 = FACE_OUTER_BOUND ( 'NONE', #7849, .T. ) ;
#9345 = CARTESIAN_POINT ( 'NONE',  ( 0.000000000000000000, 0.000000000000000000, 0.000000000000000000 ) ) ;
#9346 = AXIS2_PLACEMENT_3D ( 'NONE', #5687, #11636, #2490 ) ;
#9347 = CARTESIAN_POINT ( 'NONE',  ( -246.6527294680201408, -9.457576189692451507, 6.972573804907313821 ) ) ;
#9348 = AXIS2_PLACEMENT_3D ( 'NONE', #12358, #12287, #6423 ) ;
#9349 = ITEM_DEFINED_TRANSFORMATION ( 'NONE', 'NONE', #8913,  #805 ) ;
#9350 = VERTEX_POINT ( 'NONE', #11343 ) ;
#9351 = FACE_OUTER_BOUND ( 'NONE', #8568, .T. ) ;
#9352 = CARTESIAN_POINT ( 'NONE',  ( 0.000000000000000000, 1.438959988998140160E-15, 11.75000000000000000 ) ) ;
#9353 = ORIENTED_EDGE ( 'NONE', *, *, #10793, .F. ) ;
#9354 = ORIENTED_EDGE ( 'NONE', *, *, #12469, .T. ) ;
#9355 = CIRCLE ( 'NONE', #3594, 6.500000000000005329 ) ;
#9356 = DIRECTION ( 'NONE',  ( -0.000000000000000000, -1.000000000000000000, 0.000000000000000000 ) ) ;
#9357 = CARTESIAN_POINT ( 'NONE',  ( 3.061616997868383121E-14, 0.000000000000000000, 250.0000000000000000 ) ) ;
#9358 = CIRCLE ( 'NONE', #7015, 249.7999999999999829 ) ;
#9359 = CARTESIAN_POINT ( 'NONE',  ( -17.10461161519512174, 20.55460285096646089, 261.3381329044966606 ) ) ;
#9360 = CYLINDRICAL_SURFACE ( 'NONE', #3235, 5.500000000000005329 ) ;
#9361 = DIRECTION ( 'NONE',  ( 0.7071067811865463515, 0.000000000000000000, 0.7071067811865487940 ) ) ;
#9362 = CARTESIAN_POINT ( 'NONE',  ( -240.2602214610376450, 3.236828995589876357, 11.30545424820408229 ) ) ;
#9363 = CIRCLE ( 'NONE', #3389, 251.1999999999999886 ) ;
#9364 = ORIENTED_EDGE ( 'NONE', *, *, #8821, .F. ) ;
#9365 = CARTESIAN_POINT ( 'NONE',  ( 225.9597979674045405, 20.79694577634646535, 130.4544329367268460 ) ) ;
#9366 = VERTEX_POINT ( 'NONE', #2339 ) ;
#9367 = DIRECTION ( 'NONE',  ( -0.6368676505102706109, 0.000000000000000000, -0.7709731485165535192 ) ) ;
#9368 = ORIENTED_EDGE ( 'NONE', *, *, #42, .F. ) ;
#9369 = EDGE_LOOP ( 'NONE', ( #2550, #1545, #9416, #3963 ) ) ;
#9370 = EDGE_CURVE ( 'NONE', #808, #11582, #5602, .T. ) ;
#9371 = CARTESIAN_POINT ( 'NONE',  ( 221.6213872890270977, -30.00000000000000000, -190.2057062658400923 ) ) ;
#9372 = CARTESIAN_POINT ( 'NONE',  ( 0.000000000000000000, 19.00000000000000000, -208.0000000000000000 ) ) ;
#9373 = PRODUCT_DEFINITION_SHAPE ( 'NONE', 'NONE',  #13070 ) ;
#9374 = DIRECTION ( 'NONE',  ( 0.6368676505102708330, 0.000000000000000000, 0.7709731485165535192 ) ) ;
#9375 = DIRECTION ( 'NONE',  ( 0.000000000000000000, 0.9998057603070480415, -0.01970892327970899874 ) ) ;
#9376 = CARTESIAN_POINT ( 'NONE',  ( 0.000000000000000000, -19.00000000000000000, -230.0000000000000000 ) ) ;
#9377 = CARTESIAN_POINT ( 'NONE',  ( -247.0695545831997890, 9.592608482329058717, 7.209588857402760453 ) ) ;
#9378 = DIRECTION ( 'NONE',  ( 0.000000000000000000, 0.000000000000000000, 1.000000000000000000 ) ) ;
#9379 = AXIS2_PLACEMENT_3D ( 'NONE', #4435, #12579, #7383 ) ;
#9380 = ORIENTED_EDGE ( 'NONE', *, *, #375, .F. ) ;
#9381 = LINE ( 'NONE', #56, #3686 ) ;
#9382 = VERTEX_POINT ( 'NONE', #9472 ) ;
#9383 = DIRECTION ( 'NONE',  ( 0.6368676505102716101, 0.000000000000000000, 0.7709731485165527420 ) ) ;
#9384 = DIRECTION ( 'NONE',  ( 0.000000000000000000, 0.000000000000000000, 1.000000000000000000 ) ) ;
#9385 = AXIS2_PLACEMENT_3D ( 'NONE', #1410, #5471, #9529 ) ;
#9386 = CARTESIAN_POINT ( 'NONE',  ( 260.5542428351133140, 20.08915143297737060, -8.526617657837807229 ) ) ;
#9387 = ORIENTED_EDGE ( 'NONE', *, *, #12510, .T. ) ;
#9388 = EDGE_CURVE ( 'NONE', #5475, #8755, #347, .T. ) ;
#9389 = CARTESIAN_POINT ( 'NONE',  ( -172.3268284091859925, 20.79694577633260621, -196.4640694359954978 ) ) ;
#9390 = CARTESIAN_POINT ( 'NONE',  ( 0.000000000000000000, 30.00000000000000000, -208.0000000000000000 ) ) ;
#9391 = CARTESIAN_POINT ( 'NONE',  ( -238.8104306093018181, 0.7422746157897220920, 11.97741946070771135 ) ) ;
#9392 = CARTESIAN_POINT ( 'NONE',  ( -242.8048495217675509, -7.129644031679399419, -9.341687344795504444 ) ) ;
#9393 = AXIS2_PLACEMENT_3D ( 'NONE', #12959, #7695, #10764 ) ;
#9394 = CARTESIAN_POINT ( 'NONE',  ( 239.0427084576793959, -0.5779638303088237006, 3.452011086608069323 ) ) ;
#9395 = ADVANCED_FACE ( 'NONE', ( #12725 ), #3461, .F. ) ;
#9396 = DIRECTION ( 'NONE',  ( 0.000000000000000000, 1.000000000000000000, 0.000000000000000000 ) ) ;
#9397 = CONICAL_SURFACE ( 'NONE', #5781, 230.0000000000000000, 0.7853981633974476129 ) ;
#9398 = DIRECTION ( 'NONE',  ( -0.000000000000000000, -1.000000000000000000, 0.000000000000000000 ) ) ;
#9399 = VERTEX_POINT ( 'NONE', #2468 ) ;
#9400 = VECTOR ( 'NONE', #8042, 1000.000000000000000 ) ;
#9401 = PRODUCT_DEFINITION_SHAPE ( 'NONE', 'NONE',  #13085 ) ;
#9402 = CARTESIAN_POINT ( 'NONE',  ( 196.2980642840460064, 20.08915143284461280, 172.1812796681624889 ) ) ;
#9403 = DIRECTION ( 'NONE',  ( 0.000000000000000000, -1.000000000000000000, 0.000000000000000000 ) ) ;
#9404 = FACE_OUTER_BOUND ( 'NONE', #6616, .T. ) ;
#9405 =( REPRESENTATION_RELATIONSHIP ('NONE','NONE', #12019, #182 ) REPRESENTATION_RELATIONSHIP_WITH_TRANSFORMATION ( #7648 )SHAPE_REPRESENTATION_RELATIONSHIP( ) );
#9406 = CARTESIAN_POINT ( 'NONE',  ( -248.6772030003816667, 10.03733143285744767, 6.108624101570837794 ) ) ;
#9407 = CARTESIAN_POINT ( 'NONE',  ( 239.4470891770056653, -1.456698945183192651, -3.182458632634282303 ) ) ;
#9408 = DIRECTION ( 'NONE',  ( 0.000000000000000000, 1.000000000000000000, 0.000000000000000000 ) ) ;
#9409 = DIRECTION ( 'NONE',  ( 0.000000000000000000, 1.000000000000000000, 0.000000000000000000 ) ) ;
#9410 = DIRECTION ( 'NONE',  ( 0.000000000000000000, 0.000000000000000000, -1.000000000000000000 ) ) ;
#9411 = DIRECTION ( 'NONE',  ( -0.08715574274766177409, 0.000000000000000000, 0.9961946980917452121 ) ) ;
#9412 = EDGE_CURVE ( 'NONE', #5790, #10498, #4589, .T. ) ;
#9413 = CARTESIAN_POINT ( 'NONE',  ( 0.000000000000000000, 3.327561323230765034, 0.000000000000000000 ) ) ;
#9414 = ITEM_DEFINED_TRANSFORMATION ( 'NONE', 'NONE', #4214,  #805 ) ;
#9415 = ADVANCED_FACE ( 'NONE', ( #5667 ), #7943, .F. ) ;
#9416 = ORIENTED_EDGE ( 'NONE', *, *, #201, .T. ) ;
#9417 = AXIS2_PLACEMENT_3D ( 'NONE', #2964, #10161, #6627 ) ;
#9418 = CARTESIAN_POINT ( 'NONE',  ( 0.000000000000000000, 30.00000000000000000, 208.0000000000000000 ) ) ;
#9419 = CARTESIAN_POINT ( 'NONE',  ( 122.2593324768346008, 29.00000000000000000, 168.2755348299889988 ) ) ;
#9420 = ORIENTED_EDGE ( 'NONE', *, *, #535, .F. ) ;
#9421 = ORIENTED_EDGE ( 'NONE', *, *, #2752, .T. ) ;
#9422 = EDGE_CURVE ( 'NONE', #12785, #8105, #6252, .T. ) ;
#9423 = DIRECTION ( 'NONE',  ( 1.000000000000000000, 0.000000000000000000, 0.000000000000000000 ) ) ;
#9424 = FACE_BOUND ( 'NONE', #1841, .T. ) ;
#9425 = CIRCLE ( 'NONE', #9839, 251.5674242726969680 ) ;
#9426 = AXIS2_PLACEMENT_3D ( 'NONE', #12809, #4670, #1485 ) ;
#9427 = CARTESIAN_POINT ( 'NONE',  ( -159.4136521825795114, 20.55460285040709678, 207.7919029861446916 ) ) ;
#9428 = CARTESIAN_POINT ( 'NONE',  ( -27.68945685411286561, -18.00000000000000000, 290.6841825403027997 ) ) ;
#9429 = DIRECTION ( 'NONE',  ( 1.000000000000000000, 0.000000000000000000, 0.000000000000000000 ) ) ;
#9430 = DIRECTION ( 'NONE',  ( -0.000000000000000000, -1.000000000000000000, 0.000000000000000000 ) ) ;
#9431 = EDGE_CURVE ( 'NONE', #8298, #5214, #3868, .T. ) ;
#9432 = EDGE_LOOP ( 'NONE', ( #961, #11839, #11989, #773 ) ) ;
#9433 = CARTESIAN_POINT ( 'NONE',  ( 91.90986972409980638, 20.79694577634647246, 244.1900186690935470 ) ) ;
#9434 = EDGE_LOOP ( 'NONE', ( #230, #11647, #7301, #12087 ) ) ;
#9435 = DIRECTION ( 'NONE',  ( 0.6368676505102707219, 0.000000000000000000, 0.7709731485165535192 ) ) ;
#9436 = VERTEX_POINT ( 'NONE', #670 ) ;
#9437 = EDGE_LOOP ( 'NONE', ( #6984, #11554, #7127, #7884 ) ) ;
#9438 = VECTOR ( 'NONE', #1211, 1000.000000000000227 ) ;
#9439 = AXIS2_PLACEMENT_3D ( 'NONE', #9503, #6576, #10636 ) ;
#9440 = CARTESIAN_POINT ( 'NONE',  ( 122.2593324768346008, 19.00000000000000000, 162.7755348299889988 ) ) ;
#9441 = FACE_OUTER_BOUND ( 'NONE', #6735, .T. ) ;
#9442 = DIRECTION ( 'NONE',  ( 0.000000000000000000, 0.9998057603070481525, -0.01970892327970899874 ) ) ;
#9443 = CARTESIAN_POINT ( 'NONE',  ( -0.000000000000000000, -21.50000000000000000, 0.000000000000000000 ) ) ;
#9444 = CARTESIAN_POINT ( 'NONE',  ( -238.7110076764417670, 0.01030032076102859601, -11.74999636971691963 ) ) ;
#9445 = CARTESIAN_POINT ( 'NONE',  ( -242.2998418224646571, 6.621659878730367765, 10.00767884245070150 ) ) ;
#9446 = CONICAL_SURFACE ( 'NONE', #3685, 2.250000000000000000, 0.4188790204786335125 ) ;
#9447 = VECTOR ( 'NONE', #515, 1000.000000000000000 ) ;
#9448 = ORIENTED_EDGE ( 'NONE', *, *, #11328, .F. ) ;
#9449 = CIRCLE ( 'NONE', #3900, 5.500000000000015099 ) ;
#9450 = CARTESIAN_POINT ( 'NONE',  ( 0.000000000000000000, -19.00000000000000000, -230.0000000000000000 ) ) ;
#9451 = ORIENTED_EDGE ( 'NONE', *, *, #11276, .T. ) ;
#9452 = CARTESIAN_POINT ( 'NONE',  ( 225.1241593668336236, -19.00000000000000000, -185.9653539489990521 ) ) ;
#9453 = DIRECTION ( 'NONE',  ( -1.000000000000000000, 0.000000000000000000, 0.000000000000000000 ) ) ;
#9454 = CARTESIAN_POINT ( 'NONE',  ( 260.5542428351132571, 20.08915143297736705, 8.526617657838089670 ) ) ;
#9455 = ORIENTED_EDGE ( 'NONE', *, *, #1524, .T. ) ;
#9456 = DIRECTION ( 'NONE',  ( 0.000000000000000000, -1.000000000000000000, 0.000000000000000000 ) ) ;
#9457 = CARTESIAN_POINT ( 'NONE',  ( -241.9339721714191853, 6.203520525929971718, -10.27503750700886087 ) ) ;
#9458 = CARTESIAN_POINT ( 'NONE',  ( -238.7808081302305538, 0.6325455258416629034, 11.98332317327539798 ) ) ;
#9459 = AXIS2_PLACEMENT_3D ( 'NONE', #11542, #403, #4453 ) ;
#9460 = CARTESIAN_POINT ( 'NONE',  ( -229.6996680450366171, 1.438960022146944131E-15, 11.75000000000000000 ) ) ;
#9461 = SURFACE_STYLE_USAGE ( .BOTH. , #12460 ) ;
#9462 = APPLICATION_PROTOCOL_DEFINITION ( 'draft international standard', 'automotive_design', 1998, #9326 ) ;
#9463 = ADVANCED_FACE ( 'NONE', ( #5732 ), #2532, .T. ) ;
#9464 = DIRECTION ( 'NONE',  ( 0.000000000000000000, -0.8560027256360642767, 0.5169713083949908361 ) ) ;
#9465 = EDGE_CURVE ( 'NONE', #6828, #3384, #11864, .T. ) ;
#9466 = CARTESIAN_POINT ( 'NONE',  ( 290.6841825403032544, -19.00000000000000000, 27.68945685411186730 ) ) ;
#9467 = ORIENTED_EDGE ( 'NONE', *, *, #2809, .F. ) ;
#9468 = CARTESIAN_POINT ( 'NONE',  ( 252.8031682264634981, 19.96883746174475860, 67.71318189738019555 ) ) ;
#9469 = DIRECTION ( 'NONE',  ( 0.000000000000000000, 1.000000000000000000, 0.000000000000000000 ) ) ;
#9470 = FACE_OUTER_BOUND ( 'NONE', #6241, .T. ) ;
#9471 = CARTESIAN_POINT ( 'NONE',  ( 159.3442861576696998, -21.50000000000000000, 192.8974817588416784 ) ) ;
#9472 = CARTESIAN_POINT ( 'NONE',  ( 31.19222893192146273, -19.00000000000000000, -286.4438302234615890 ) ) ;
#9473 = DIRECTION ( 'NONE',  ( 0.9063077870366496036, 0.000000000000000000, 0.4226182617407002740 ) ) ;
#9474 = DIRECTION ( 'NONE',  ( 0.000000000000000000, -1.000000000000000000, 0.000000000000000000 ) ) ;
#9475 = CONTEXT_DEPENDENT_SHAPE_REPRESENTATION ( #1508, #3212 ) ;
#9476 = DIRECTION ( 'NONE',  ( 8.659560562354913137E-17, -0.7071067811865489050, 0.7071067811865460184 ) ) ;
#9477 = STYLED_ITEM ( 'NONE', ( #3313 ), #5959 ) ;
#9478 =( REPRESENTATION_RELATIONSHIP ('NONE','NONE', #12019, #5191 ) REPRESENTATION_RELATIONSHIP_WITH_TRANSFORMATION ( #11813 )SHAPE_REPRESENTATION_RELATIONSHIP( ) );
#9479 = PRODUCT_DEFINITION_SHAPE ( 'NONE', 'NONE',  #13045 ) ;
#9480 = CARTESIAN_POINT ( 'NONE',  ( -229.9520201725233619, -11.04255732478361729, 4.700793194709331324 ) ) ;
#9481 = ORIENTED_EDGE ( 'NONE', *, *, #12395, .F. ) ;
#9482 = ORIENTED_EDGE ( 'NONE', *, *, #5328, .F. ) ;
#9483 = DIRECTION ( 'NONE',  ( 0.000000000000000000, 1.000000000000000000, 0.000000000000000000 ) ) ;
#9484 = CARTESIAN_POINT ( 'NONE',  ( 197.8197553893915028, 19.00000000000000000, -58.77553482998990830 ) ) ;
#9485 = EDGE_CURVE ( 'NONE', #7994, #11942, #10794, .T. ) ;
#9486 = EDGE_CURVE ( 'NONE', #11239, #9649, #9717, .T. ) ;
#9487 = CARTESIAN_POINT ( 'NONE',  ( -234.8993005735983104, 20.55460285152947009, -115.8123742918138248 ) ) ;
#9488 = VECTOR ( 'NONE', #12881, 1000.000000000000114 ) ;
#9489 = DIRECTION ( 'NONE',  ( 0.000000000000000000, -1.000000000000000000, 0.000000000000000000 ) ) ;
#9490 = DIRECTION ( 'NONE',  ( -0.9961946980917459893, 0.000000000000000000, 0.08715574274765504337 ) ) ;
#9491 = LINE ( 'NONE', #10494, #3689 ) ;
#9492 = DIRECTION ( 'NONE',  ( 8.659560562354963673E-17, 0.7071067811865450192, -0.7071067811865500152 ) ) ;
#9493 = EDGE_LOOP ( 'NONE', ( #11667, #2737, #8171, #2032 ) ) ;
#9494 = DIRECTION ( 'NONE',  ( 1.000000000000000000, 0.000000000000000000, 0.000000000000000000 ) ) ;
#9495 = VERTEX_POINT ( 'NONE', #476 ) ;
#9496 = ORIENTED_EDGE ( 'NONE', *, *, #6227, .T. ) ;
#9497 = ORIENTED_EDGE ( 'NONE', *, *, #12557, .F. ) ;
#9498 = CARTESIAN_POINT ( 'NONE',  ( 6.345753394971347358E-13, 20.08915143297736350, -260.5542428351130866 ) ) ;
#9499 = ADVANCED_FACE ( 'NONE', ( #2713 ), #8561, .T. ) ;
#9500 = CARTESIAN_POINT ( 'NONE',  ( 0.000000000000000000, 19.00000000000000000, -195.0000000000000000 ) ) ;
#9501 = CARTESIAN_POINT ( 'NONE',  ( 239.1299809604698794, 0.8683754746916950706, -3.391597751417305240 ) ) ;
#9502 = CARTESIAN_POINT ( 'NONE',  ( -238.9888240692591239, 1.140781236982990166, -11.69457573833076758 ) ) ;
#9503 = CARTESIAN_POINT ( 'NONE',  ( 71.82423009839129691, 30.00000000000000000, 197.3354503650404865 ) ) ;
#9504 = ADVANCED_FACE ( 'NONE', ( #4721 ), #2386, .F. ) ;
#9505 = ITEM_DEFINED_TRANSFORMATION ( 'NONE', 'NONE', #8689,  #805 ) ;
#9506 = ORIENTED_EDGE ( 'NONE', *, *, #6294, .T. ) ;
#9507 = CARTESIAN_POINT ( 'NONE',  ( 159.9811538081800109, -30.00000000000000000, 193.6684549073582673 ) ) ;
#9508 = VERTEX_POINT ( 'NONE', #9591 ) ;
#9509 = CYLINDRICAL_SURFACE ( 'NONE', #614, 250.1999999999999602 ) ;
#9510 = DIRECTION ( 'NONE',  ( 0.6368676505102707219, 0.000000000000000000, 0.7709731485165536302 ) ) ;
#9511 = CARTESIAN_POINT ( 'NONE',  ( 257.2112267038638151, 20.08915143297736350, -42.46883004693691532 ) ) ;
#9512 = CARTESIAN_POINT ( 'NONE',  ( 0.000000000000000000, -25.00000000000000000, 0.000000000000000000 ) ) ;
#9513 = CARTESIAN_POINT ( 'NONE',  ( -240.0746691521900118, 2.719637366898895348, -11.70176364693860904 ) ) ;
#9514 = CARTESIAN_POINT ( 'NONE',  ( -239.3224710781300644, 1.645298538954363066, 11.88664485503670853 ) ) ;
#9515 = APPLICATION_CONTEXT ( 'automotive_design' ) ;
#9516 = DIRECTION ( 'NONE',  ( 0.6368676505102707219, 0.000000000000000000, 0.7709731485165536302 ) ) ;
#9517 = CARTESIAN_POINT ( 'NONE',  ( 122.2593324768334071, 30.00000000000000000, -168.2755348299895104 ) ) ;
#9518 = CARTESIAN_POINT ( 'NONE',  ( -229.9295651076812135, 10.57170285972954815, -5.726701700993176658 ) ) ;
#9519 = DIRECTION ( 'NONE',  ( 1.000000000000000000, 0.000000000000000000, 0.000000000000000000 ) ) ;
#9520 = ORIENTED_EDGE ( 'NONE', *, *, #8745, .T. ) ;
#9521 = AXIS2_PLACEMENT_3D ( 'NONE', #3906, #583, #11978 ) ;
#9522 = CARTESIAN_POINT ( 'NONE',  ( -115.7315435907638346, 19.96883745872212046, 234.7354397761344273 ) ) ;
#9523 = DIRECTION ( 'NONE',  ( 0.000000000000000000, 1.000000000000000000, 0.000000000000000000 ) ) ;
#9524 = DIRECTION ( 'NONE',  ( 0.6368676505102690566, 0.000000000000000000, 0.7709731485165549625 ) ) ;
#9525 = EDGE_CURVE ( 'NONE', #1949, #7844, #4654, .T. ) ;
#9526 = CARTESIAN_POINT ( 'NONE',  ( 7.960204194457791533E-16, 18.00000000000000000, -201.4999999999999716 ) ) ;
#9527 = CARTESIAN_POINT ( 'NONE',  ( -206.8203823583193639, 20.08915143297736350, 158.7026972336029758 ) ) ;
#9528 = FACE_OUTER_BOUND ( 'NONE', #7788, .T. ) ;
#9529 = DIRECTION ( 'NONE',  ( -0.5000000000000039968, 0.000000000000000000, 0.8660254037844362651 ) ) ;
#9530 = CARTESIAN_POINT ( 'NONE',  ( -246.5915682055979801, -9.436693423004101078, 7.000847393551240749 ) ) ;
#9531 = CARTESIAN_POINT ( 'NONE',  ( 240.5112511684797880, -3.170498834991128945, -1.486196988779163952 ) ) ;
#9532 = CARTESIAN_POINT ( 'NONE',  ( 1.091807554230414677E-12, 20.55460285106647689, -261.3381329044966606 ) ) ;
#9533 = ORIENTED_EDGE ( 'NONE', *, *, #3823, .F. ) ;
#9534 = ORIENTED_EDGE ( 'NONE', *, *, #8077, .F. ) ;
#9535 = DIRECTION ( 'NONE',  ( 0.000000000000000000, 0.000000000000000000, 1.000000000000000000 ) ) ;
#9536 = DIRECTION ( 'NONE',  ( 0.6368676505102716101, 0.000000000000000000, 0.7709731485165527420 ) ) ;
#9537 = AXIS2_PLACEMENT_3D ( 'NONE', #8743, #1940, #9874 ) ;
#9538 = EDGE_CURVE ( 'NONE', #1045, #9651, #12794, .T. ) ;
#9539 = AXIS2_PLACEMENT_3D ( 'NONE', #11628, #620, #6758 ) ;
#9540 = CARTESIAN_POINT ( 'NONE',  ( 17.10461161403171815, 20.55460285106647689, -261.3381329044966606 ) ) ;
#9541 = DIRECTION ( 'NONE',  ( -0.000000000000000000, -1.000000000000000000, 0.000000000000000000 ) ) ;
#9542 = CARTESIAN_POINT ( 'NONE',  ( 0.000000000000000000, 0.000000000000000000, 0.000000000000000000 ) ) ;
#9543 = DIRECTION ( 'NONE',  ( 0.6368676505102716101, 0.000000000000000000, 0.7709731485165527420 ) ) ;
#9544 = CARTESIAN_POINT ( 'NONE',  ( -91.90986972410016165, 20.79694577634646890, 244.1900186690933765 ) ) ;
#9545 = EDGE_LOOP ( 'NONE', ( #2485, #2146, #4430, #9083 ) ) ;
#9546 = CARTESIAN_POINT ( 'NONE',  ( 206.9952515782969158, 20.79694577634646890, -158.8368823490023374 ) ) ;
#9547 = EDGE_CURVE ( 'NONE', #6775, #8308, #1533, .T. ) ;
#9549 = ORIENTED_EDGE ( 'NONE', *, *, #4107, .T. ) ;
#9548 = AXIS2_PLACEMENT_3D ( 'NONE', #8202, #3112, #7189 ) ;
#9550 = ADVANCED_FACE ( 'NONE', ( #7728 ), #5140, .F. ) ;
#9551 = DIRECTION ( 'NONE',  ( 0.000000000000000000, 1.000000000000000000, 0.000000000000000000 ) ) ;
#9552 = ORIENTED_EDGE ( 'NONE', *, *, #12657, .F. ) ;
#9553 = ORIENTED_EDGE ( 'NONE', *, *, #9202, .T. ) ;
#9554 = CIRCLE ( 'NONE', #9132, 6.500000000000005329 ) ;
#9555 = AXIS2_PLACEMENT_3D ( 'NONE', #3449, #9398, #4581 ) ;
#9556 = CARTESIAN_POINT ( 'NONE',  ( 197.8197553893920144, 29.00000000000000000, 64.27553482998850143 ) ) ;
#9557 = DIRECTION ( 'NONE',  ( -0.6368676505102706109, 0.000000000000000000, -0.7709731485165535192 ) ) ;
#9558 = DIRECTION ( 'NONE',  ( 0.000000000000000000, 1.000000000000000000, 0.000000000000000000 ) ) ;
#9559 = CIRCLE ( 'NONE', #8079, 6.500000000000005329 ) ;
#9560 = DIRECTION ( 'NONE',  ( 0.000000000000000000, 1.000000000000000000, 0.000000000000000000 ) ) ;
#9561 = CARTESIAN_POINT ( 'NONE',  ( 3.056106087272219914E-14, 22.00000000000000000, 249.2999999999999829 ) ) ;
#9562 = SURFACE_SIDE_STYLE ('',( #1574 ) ) ;
#9563 = ORIENTED_EDGE ( 'NONE', *, *, #755, .T. ) ;
#9564 = CYLINDRICAL_SURFACE ( 'NONE', #11580, 2.749999999999999556 ) ;
#9565 = ADVANCED_FACE ( 'NONE', ( #3728 ), #7794, .F. ) ;
#9566 = EDGE_LOOP ( 'NONE', ( #9952, #467 ) ) ;
#9567 = EDGE_CURVE ( 'NONE', #354, #10034, #4086, .T. ) ;
#9568 =( REPRESENTATION_RELATIONSHIP ('NONE','NONE', #12019, #182 ) REPRESENTATION_RELATIONSHIP_WITH_TRANSFORMATION ( #11382 )SHAPE_REPRESENTATION_RELATIONSHIP( ) );
#9569 = DIRECTION ( 'NONE',  ( 0.000000000000000000, 1.000000000000000000, 0.000000000000000000 ) ) ;
#9570 = CARTESIAN_POINT ( 'NONE',  ( -210.0000000000000000, 30.00000000000000000, 0.000000000000000000 ) ) ;
#9571 = VECTOR ( 'NONE', #344, 1000.000000000000114 ) ;
#9572 = AXIS2_PLACEMENT_3D ( 'NONE', #7580, #520, #9634 ) ;
#9573 = ADVANCED_FACE ( 'NONE', ( #7173 ), #4934, .F. ) ;
#9574 = CARTESIAN_POINT ( 'NONE',  ( -27.68945685411286561, -29.00000000000000000, 290.6841825403027997 ) ) ;
#9575 = CARTESIAN_POINT ( 'NONE',  ( 290.6841825403032544, -30.00000000000000000, 27.68945685411186730 ) ) ;
#9576 = CYLINDRICAL_SURFACE ( 'NONE', #1689, 5.500000000000015099 ) ;
#9577 = CARTESIAN_POINT ( 'NONE',  ( -229.7832113950239545, 6.204037592689317648, 9.986088990952895372 ) ) ;
#9578 = DIRECTION ( 'NONE',  ( 0.000000000000000000, -1.000000000000000000, 0.000000000000000000 ) ) ;
#9579 = SHAPE_DEFINITION_REPRESENTATION ( #1793, #182 ) ;
#9580 = DIRECTION ( 'NONE',  ( 0.6368676505102716101, 0.000000000000000000, 0.7709731485165527420 ) ) ;
#9581 = AXIS2_PLACEMENT_3D ( 'NONE', #2913, #72, #8208 ) ;
#9582 = VECTOR ( 'NONE', #9453, 1000.000000000000000 ) ;
#9583 = LINE ( 'NONE', #4514, #8505 ) ;
#9584 = EDGE_LOOP ( 'NONE', ( #78, #5700, #6730, #1861 ) ) ;
#9585 = CARTESIAN_POINT ( 'NONE',  ( 234.7354397747064354, 19.96883745941838484, 115.7315435904383349 ) ) ;
#9586 = LINE ( 'NONE', #8278, #11594 ) ;
#9587 = CARTESIAN_POINT ( 'NONE',  ( -197.8197553893924976, 18.00000000000000000, -70.77553482998720824 ) ) ;
#9588 = DIRECTION ( 'NONE',  ( 0.4503334343941817752, -0.7071067811865080488, 0.5451603414288286320 ) ) ;
#9589 = DIRECTION ( 'NONE',  ( 0.000000000000000000, -1.000000000000000000, 0.000000000000000000 ) ) ;
#9590 = CARTESIAN_POINT ( 'NONE',  ( -8.526617657838487574, 20.08915143297736705, 260.5542428351131434 ) ) ;
#9591 = CARTESIAN_POINT ( 'NONE',  ( 165.3358371128624924, 2.772967769358929857, 200.1506762031210371 ) ) ;
#9592 = DIRECTION ( 'NONE',  ( -0.7545873610930013964, 0.5538822189107471816, -0.3518698652246416980 ) ) ;
#9593 = CARTESIAN_POINT ( 'NONE',  ( 229.9733680233431130, 4.286263893147487610E-16, -3.499999999999964917 ) ) ;
#9594 = CARTESIAN_POINT ( 'NONE',  ( 0.000000000000000000, 11.79660968244690089, 249.7999999999999829 ) ) ;
#9595 = EDGE_CURVE ( 'NONE', #2165, #5446, #2588, .T. ) ;
#9596 = AXIS2_PLACEMENT_3D ( 'NONE', #9837, #12773, #5577 ) ;
#9597 = DIRECTION ( 'NONE',  ( -1.000000000000000000, -0.000000000000000000, -0.000000000000000000 ) ) ;
#9598 = DIRECTION ( 'NONE',  ( 0.000000000000000000, 1.000000000000000000, 0.000000000000000000 ) ) ;
#9599 = ORIENTED_EDGE ( 'NONE', *, *, #6008, .F. ) ;
#9600 = ORIENTED_EDGE ( 'NONE', *, *, #5789, .T. ) ;
#9601 = CARTESIAN_POINT ( 'NONE',  ( 0.000000000000000000, -23.50000000000000000, 0.000000000000000000 ) ) ;
#9602 = DIRECTION ( 'NONE',  ( 0.000000000000000000, 0.000000000000000000, -1.000000000000000000 ) ) ;
#9603 = CARTESIAN_POINT ( 'NONE',  ( -17.10461161402953323, 20.55460285106647689, -261.3381329044966606 ) ) ;
#9604 = DIRECTION ( 'NONE',  ( 0.000000000000000000, 0.9998057603070480415, -0.01970892327970899874 ) ) ;
#9605 = PRODUCT_DEFINITION_SHAPE ( 'NONE', 'NONE',  #13176 ) ;
#9606 = CARTESIAN_POINT ( 'NONE',  ( 0.000000000000000000, 0.000000000000000000, 0.000000000000000000 ) ) ;
#9607 = DIRECTION ( 'NONE',  ( 0.000000000000000000, 0.9998057603070480415, -0.01970892327970899874 ) ) ;
#9608 = CONICAL_SURFACE ( 'NONE', #11758, 3.000000000000000000, 0.7853981633974490562 ) ;
#9609 = CARTESIAN_POINT ( 'NONE',  ( -260.3553053170167004, 20.79694577634646535, 17.06764083276396704 ) ) ;
#9610 = VERTEX_POINT ( 'NONE', #8114 ) ;
#9611 = ADVANCED_FACE ( 'NONE', ( #8044 ), #3224, .T. ) ;
#9612 = CARTESIAN_POINT ( 'NONE',  ( 260.7745447061712412, 20.79694577634646890, -8.533827019709542938 ) ) ;
#9613 = ADVANCED_FACE ( 'NONE', ( #11309 ), #11173, .F. ) ;
#9614 = VERTEX_POINT ( 'NONE', #2040 ) ;
#9615 = LINE ( 'NONE', #2673, #616 ) ;
#9616 = ORIENTED_EDGE ( 'NONE', *, *, #11939, .T. ) ;
#9617 = ORIENTED_EDGE ( 'NONE', *, *, #6818, .F. ) ;
#9618 = AXIS2_PLACEMENT_3D ( 'NONE', #610, #3535, #2537 ) ;
#9619 = LINE ( 'NONE', #10503, #5829 ) ;
#9620 = CARTESIAN_POINT ( 'NONE',  ( -239.9867712987582706, 2.433335514366328667, -11.49559079283426755 ) ) ;
#9621 = CONICAL_SURFACE ( 'NONE', #11974, 6.500000000000005329, 0.7853981633974518317 ) ;
#9622 = EDGE_CURVE ( 'NONE', #10706, #8254, #12392, .T. ) ;
#9623 = LINE ( 'NONE', #6444, #3442 ) ;
#9624 = CARTESIAN_POINT ( 'NONE',  ( 0.000000000000000000, -3.327561323230890267, 238.4705882352940307 ) ) ;
#9625 = LINE ( 'NONE', #2563, #6245 ) ;
#9626 = CONTEXT_DEPENDENT_SHAPE_REPRESENTATION ( #726, #4136 ) ;
#9627 = EDGE_LOOP ( 'NONE', ( #10307, #111, #9968, #766 ) ) ;
#9628 = DIRECTION ( 'NONE',  ( 0.000000000000000000, -0.9998057603070481525, 0.01970892327970899874 ) ) ;
#9629 = AXIS2_PLACEMENT_3D ( 'NONE', #279, #3127, #7211 ) ;
#9630 = ORIENTED_EDGE ( 'NONE', *, *, #11829, .T. ) ;
#9631 = VECTOR ( 'NONE', #2817, 1000.000000000000000 ) ;
#9632 = CARTESIAN_POINT ( 'NONE',  ( -130.7196491263533744, -20.69999999999999929, 200.0834159351620656 ) ) ;
#9633 = DIRECTION ( 'NONE',  ( 0.000000000000000000, 1.000000000000000000, 0.000000000000000000 ) ) ;
#9634 = DIRECTION ( 'NONE',  ( 0.000000000000000000, 0.000000000000000000, -1.000000000000000000 ) ) ;
#9635 = DIRECTION ( 'NONE',  ( 0.000000000000000000, -0.01970892327970900221, -0.9998057603070482635 ) ) ;
#9636 = CARTESIAN_POINT ( 'NONE',  ( -239.4202119743104902, 1.749723677800394839, 11.87175088374991994 ) ) ;
#9638 = EDGE_CURVE ( 'NONE', #11029, #10530, #9044, .T. ) ;
#9637 = VECTOR ( 'NONE', #11611, 1000.000000000000000 ) ;
#9639 = AXIS2_PLACEMENT_3D ( 'NONE', #9556, #11435, #1498 ) ;
#9640 = CARTESIAN_POINT ( 'NONE',  ( 71.82423009839129691, 30.00000000000000000, 203.8354503650404865 ) ) ;
#9641 = EDGE_CURVE ( 'NONE', #12027, #1246, #6109, .T. ) ;
#9642 = CIRCLE ( 'NONE', #5821, 2.749999999999999556 ) ;
#9643 = CARTESIAN_POINT ( 'NONE',  ( -248.8440518477580667, -9.943161799024673897, 6.718187330855736938 ) ) ;
#9644 = DIRECTION ( 'NONE',  ( -0.000000000000000000, -1.000000000000000000, 0.000000000000000000 ) ) ;
#9645 = AXIS2_PLACEMENT_3D ( 'NONE', #4665, #3804, #2794 ) ;
#9646 = DIRECTION ( 'NONE',  ( 0.1445786100687990738, 0.5538822189107471816, 0.8199460427888418668 ) ) ;
#9647 = CARTESIAN_POINT ( 'NONE',  ( -229.9519813856196606, 11.04228730818343251, 4.712348903618373441 ) ) ;
#9648 = CONTEXT_DEPENDENT_SHAPE_REPRESENTATION ( #11756, #4392 ) ;
#9649 = VERTEX_POINT ( 'NONE', #1977 ) ;
#9650 = VECTOR ( 'NONE', #3760, 1000.000000000000000 ) ;
#9651 = VERTEX_POINT ( 'NONE', #10233 ) ;
#9652 = CARTESIAN_POINT ( 'NONE',  ( -122.2593324768359935, 30.00000000000000000, -168.2755348299880040 ) ) ;
#9653 = VERTEX_POINT ( 'NONE', #5163 ) ;
#9654 = CARTESIAN_POINT ( 'NONE',  ( -172.5787240286020392, 19.96883746144090210, 196.7513681798772609 ) ) ;
#9655 = CARTESIAN_POINT ( 'NONE',  ( -229.6996680450365034, 7.200459016985159977E-17, -11.75000000000000000 ) ) ;
#9656 = CYLINDRICAL_SURFACE ( 'NONE', #9868, 5.500000000000015099 ) ;
#9657 = CARTESIAN_POINT ( 'NONE',  ( -1.009183486025028462E-12, 20.55460285106647689, 261.3381329044966606 ) ) ;
#9658 = EDGE_CURVE ( 'NONE', #368, #1401, #1326, .T. ) ;
#9659 = CARTESIAN_POINT ( 'NONE',  ( -240.4404613007375815, 3.704209566697797662, 11.41407139955384764 ) ) ;
#9660 = VECTOR ( 'NONE', #9896, 1000.000000000000000 ) ;
#9661 = CARTESIAN_POINT ( 'NONE',  ( 3.059167704270088292E-14, 0.000000000000000000, 249.7999999999999829 ) ) ;
#9662 = CARTESIAN_POINT ( 'NONE',  ( -40.42519547187234963, -138.4705547276867321, 10.83189848055834936 ) ) ;
#9663 = CARTESIAN_POINT ( 'NONE',  ( -7.780566028168587395E-13, 20.08915143297736350, 260.5542428351130866 ) ) ;
#9664 = CONTEXT_DEPENDENT_SHAPE_REPRESENTATION ( #12060, #8890 ) ;
#9665 = CARTESIAN_POINT ( 'NONE',  ( -240.5991998574518220, -4.074980142339518885, -11.29000475009753579 ) ) ;
#9666 = CARTESIAN_POINT ( 'NONE',  ( -122.2593324768321992, 19.00000000000000000, 168.2755348299905052 ) ) ;
#9667 = ORIENTED_EDGE ( 'NONE', *, *, #1901, .T. ) ;
#9668 = ORIENTED_EDGE ( 'NONE', *, *, #10293, .F. ) ;
#9669 = AXIS2_PLACEMENT_3D ( 'NONE', #637, #1573, #3558 ) ;
#9670 = CIRCLE ( 'NONE', #8206, 5.499999999999986677 ) ;
#9671 = CARTESIAN_POINT ( 'NONE',  ( 0.000000000000000000, -2.772967769359314882, 0.000000000000000000 ) ) ;
#9672 = DIRECTION ( 'NONE',  ( 0.6368676505102716101, 0.000000000000000000, 0.7709731485165527420 ) ) ;
#9673 = CARTESIAN_POINT ( 'NONE',  ( -207.3438552930580272, 20.79694577641581077, -159.0697709843959728 ) ) ;
#9674 = FACE_OUTER_BOUND ( 'NONE', #2199, .T. ) ;
#9675 = DIRECTION ( 'NONE',  ( -0.7660444431189749048, 0.000000000000000000, -0.6427876096865430267 ) ) ;
#9676 = CARTESIAN_POINT ( 'NONE',  ( -194.2446334056325270, -29.00000000000000000, -235.1468102975487682 ) ) ;
#9677 = DIRECTION ( 'NONE',  ( 0.000000000000000000, 0.000000000000000000, 1.000000000000000000 ) ) ;
#9678 = CONICAL_SURFACE ( 'NONE', #1391, 195.0000000000000000, 0.7853981633974476129 ) ;
#9679 = ORIENTED_EDGE ( 'NONE', *, *, #11690, .F. ) ;
#9680 = ORIENTED_EDGE ( 'NONE', *, *, #2456, .T. ) ;
#9681 = CARTESIAN_POINT ( 'NONE',  ( 71.82423009839129691, 30.00000000000000000, -190.8354503650404865 ) ) ;
#9682 = EDGE_LOOP ( 'NONE', ( #10831, #8688, #1857, #3059 ) ) ;
#9683 = ORIENTED_EDGE ( 'NONE', *, *, #3286, .F. ) ;
#9684 = ORIENTED_EDGE ( 'NONE', *, *, #2892, .F. ) ;
#9685 = AXIS2_PLACEMENT_3D ( 'NONE', #5713, #1590, #10779 ) ;
#9686 = CARTESIAN_POINT ( 'NONE',  ( 0.000000000000000000, 9.830508068689120194, 0.000000000000000000 ) ) ;
#9687 = CARTESIAN_POINT ( 'NONE',  ( -239.9440496357930499, 2.353898415756322304, -11.51208791644674001 ) ) ;
#9688 = ADVANCED_FACE ( 'NONE', ( #10105 ), #10478, .F. ) ;
#9689 = EDGE_CURVE ( 'NONE', #6909, #12416, #2100, .T. ) ;
#9690 = CARTESIAN_POINT ( 'NONE',  ( 17.05314194221880086, 20.08915143297735284, -260.5542428351129729 ) ) ;
#9691 = CARTESIAN_POINT ( 'NONE',  ( -197.8197553893924976, 30.00000000000000000, -64.27553482998719403 ) ) ;
#9692 = VERTEX_POINT ( 'NONE', #4103 ) ;
#9693 = DIRECTION ( 'NONE',  ( 0.000000000000000000, 0.000000000000000000, 1.000000000000000000 ) ) ;
#9694 = ORIENTED_EDGE ( 'NONE', *, *, #9388, .F. ) ;
#9695 = CARTESIAN_POINT ( 'NONE',  ( -241.5622318768846810, 5.708434624212912922, -10.27645530435382426 ) ) ;
#9696 = PRODUCT_RELATED_PRODUCT_CATEGORY ( 'part', '', ( #6399 ) ) ;
#9697 = CARTESIAN_POINT ( 'NONE',  ( -250.0000000000000000, 0.000000000000000000, 0.000000000000000000 ) ) ;
#9698 = CARTESIAN_POINT ( 'NONE',  ( -229.6889200636375108, -1.000000000000000000, -11.95826074310140008 ) ) ;
#9699 = DIRECTION ( 'NONE',  ( 0.000000000000000000, 0.000000000000000000, -1.000000000000000000 ) ) ;
#9700 = CARTESIAN_POINT ( 'NONE',  ( -229.7307169744397584, 3.794695336103924177, -11.12700569152495689 ) ) ;
#9701 = DIRECTION ( 'NONE',  ( 1.000000000000000000, 0.000000000000000000, 0.000000000000000000 ) ) ;
#9702 = DIRECTION ( 'NONE',  ( 0.000000000000000000, 1.000000000000000000, 0.000000000000000000 ) ) ;
#9703 = CONTEXT_DEPENDENT_SHAPE_REPRESENTATION ( #8718, #9479 ) ;
#9704 = CARTESIAN_POINT ( 'NONE',  ( -289.8128292627096130, -30.00000000000000000, 10.41748504886635907 ) ) ;
#9705 = CONTEXT_DEPENDENT_SHAPE_REPRESENTATION ( #2630, #2481 ) ;
#9706 = ORIENTED_EDGE ( 'NONE', *, *, #870, .F. ) ;
#9707 = ADVANCED_FACE ( 'NONE', ( #9242 ), #9608, .F. ) ;
#9708 = ORIENTED_EDGE ( 'NONE', *, *, #2203, .T. ) ;
#9709 = EDGE_CURVE ( 'NONE', #1760, #2672, #12375, .T. ) ;
#9710 = CARTESIAN_POINT ( 'NONE',  ( -249.1360723393657395, -10.36505329229039596, -5.534757211193051418 ) ) ;
#9711 = ORIENTED_EDGE ( 'NONE', *, *, #11172, .T. ) ;
#9712 = CARTESIAN_POINT ( 'NONE',  ( -196.7513681794031868, 19.96883746182613706, -172.5787240283650590 ) ) ;
#9713 = CARTESIAN_POINT ( 'NONE',  ( 0.000000000000000000, 25.50000000000000000, 249.7999999999999545 ) ) ;
#9714 = DIRECTION ( 'NONE',  ( 0.000000000000000000, 0.000000000000000000, 1.000000000000000000 ) ) ;
#9715 = DIRECTION ( 'NONE',  ( 0.000000000000000000, 0.000000000000000000, -1.000000000000000000 ) ) ;
#9716 = DIRECTION ( 'NONE',  ( -0.6368676505102708330, 0.000000000000000000, -0.7709731485165536302 ) ) ;
#9717 = LINE ( 'NONE', #8543, #11114 ) ;
#9718 = DIRECTION ( 'NONE',  ( -0.7660444431189813441, 0.000000000000000000, 0.6427876096865353661 ) ) ;
#9719 = CARTESIAN_POINT ( 'NONE',  ( 229.9750438049949537, 0.9064452134480361911, -3.388396133414032896 ) ) ;
#9720 = CONTEXT_DEPENDENT_SHAPE_REPRESENTATION ( #829, #10163 ) ;
#9721 = PRODUCT_DEFINITION_SHAPE ( 'NONE', 'NONE',  #13143 ) ;
#9722 = CARTESIAN_POINT ( 'NONE',  ( -249.7544427809737613, 11.44486579037191554, 2.664765662472057262 ) ) ;
#9723 = CARTESIAN_POINT ( 'NONE',  ( 0.000000000000000000, -22.00000000000000000, 0.000000000000000000 ) ) ;
#9724 = VECTOR ( 'NONE', #2777, 1000.000000000000000 ) ;
#9725 = EDGE_CURVE ( 'NONE', #8298, #5907, #5032, .T. ) ;
#9726 = CARTESIAN_POINT ( 'NONE',  ( -229.6989920831166216, -2.478440081108693516, 11.76488731315652636 ) ) ;
#9727 = ORIENTED_EDGE ( 'NONE', *, *, #10382, .F. ) ;
#9728 = ORIENTED_EDGE ( 'NONE', *, *, #7056, .T. ) ;
#9729 = DIRECTION ( 'NONE',  ( -1.000000000000000000, 0.000000000000000000, 0.000000000000000000 ) ) ;
#9730 = FACE_BOUND ( 'NONE', #1333, .T. ) ;
#9731 = EDGE_CURVE ( 'NONE', #3634, #3738, #7703, .T. ) ;
#9732 = CARTESIAN_POINT ( 'NONE',  ( -259.0935598604214647, 20.79694577620453799, 34.13493237032840000 ) ) ;
#9733 = AXIS2_PLACEMENT_3D ( 'NONE', #12292, #6099, #10150 ) ;
#9734 = DIRECTION ( 'NONE',  ( 0.000000000000000000, 1.000000000000000000, 0.000000000000000000 ) ) ;
#9735 = DIRECTION ( 'NONE',  ( 0.9063077870366540445, 0.000000000000000000, -0.4226182617406912256 ) ) ;
#9736 = CARTESIAN_POINT ( 'NONE',  ( 0.000000000000000000, -3.327561323230890267, 0.000000000000000000 ) ) ;
#9737 = CARTESIAN_POINT ( 'NONE',  ( -233.0000000000000000, 0.000000000000000000, 0.000000000000000000 ) ) ;
#9738 = ORIENTED_EDGE ( 'NONE', *, *, #10196, .F. ) ;
#9739 = CARTESIAN_POINT ( 'NONE',  ( -122.2593324768321992, 30.00000000000000000, 168.2755348299905052 ) ) ;
#9740 = ORIENTED_EDGE ( 'NONE', *, *, #521, .T. ) ;
#9741 = ORIENTED_EDGE ( 'NONE', *, *, #3248, .F. ) ;
#9742 = AXIS2_PLACEMENT_3D ( 'NONE', #6951, #11007, #8817 ) ;
#9743 = CARTESIAN_POINT ( 'NONE',  ( 151.8458048843644690, 20.08915143297736705, 211.9058003148607270 ) ) ;
#9744 = ORIENTED_EDGE ( 'NONE', *, *, #59, .F. ) ;
#9745 = DIRECTION ( 'NONE',  ( 0.000000000000000000, 1.000000000000000000, 0.000000000000000000 ) ) ;
#9746 = DIRECTION ( 'NONE',  ( -0.000000000000000000, -1.000000000000000000, 0.000000000000000000 ) ) ;
#9747 =( REPRESENTATION_RELATIONSHIP ('NONE','NONE', #12019, #182 ) REPRESENTATION_RELATIONSHIP_WITH_TRANSFORMATION ( #7153 )SHAPE_REPRESENTATION_RELATIONSHIP( ) );
#9748 = CARTESIAN_POINT ( 'NONE',  ( 122.2593324768334071, 29.00000000000000000, -168.2755348299895104 ) ) ;
#9749 = DIRECTION ( 'NONE',  ( 0.000000000000000000, -1.000000000000000000, 0.000000000000000000 ) ) ;
#9750 =( LENGTH_UNIT ( ) NAMED_UNIT ( * ) SI_UNIT ( .MILLI., .METRE. ) );
#9751 = CARTESIAN_POINT ( 'NONE',  ( -248.0831933713610056, 9.830508068705238856, 6.436117704883899115 ) ) ;
#9752 = CIRCLE ( 'NONE', #11471, 5.500000000000015099 ) ;
#9753 = PRODUCT_DEFINITION_SHAPE ( 'NONE', 'NONE',  #13061 ) ;
#9754 = VECTOR ( 'NONE', #11121, 1000.000000000000000 ) ;
#9755 = ITEM_DEFINED_TRANSFORMATION ( 'NONE', 'NONE', #1878,  #805 ) ;
#9756 = EDGE_LOOP ( 'NONE', ( #4326, #2632, #4869, #9496 ) ) ;
#9757 = AXIS2_PLACEMENT_3D ( 'NONE', #12284, #93, #12418 ) ;
#9758 = DIRECTION ( 'NONE',  ( 0.000000000000000000, 1.000000000000000000, 0.000000000000000000 ) ) ;
#9759 = CIRCLE ( 'NONE', #12740, 260.1830065359559967 ) ;
#9760 = ORIENTED_EDGE ( 'NONE', *, *, #790, .F. ) ;
#9761 = CARTESIAN_POINT ( 'NONE',  ( -242.4218346718328974, 6.744440870307020219, -9.622654846098170012 ) ) ;
#9762 = ORIENTED_EDGE ( 'NONE', *, *, #8649, .F. ) ;
#9763 = CIRCLE ( 'NONE', #11046, 5.500000000000005329 ) ;
#9764 = CONICAL_SURFACE ( 'NONE', #413, 5.499999999999986677, 0.7853981633974461696 ) ;
#9765 = ADVANCED_FACE ( 'NONE', ( #12245 ), #3098, .F. ) ;
#9766 = CARTESIAN_POINT ( 'NONE',  ( 24.18668477630849978, -29.00000000000000000, -294.9245348571436693 ) ) ;
#9767 = DIRECTION ( 'NONE',  ( 0.000000000000000000, 1.000000000000000000, 0.000000000000000000 ) ) ;
#9768 = CARTESIAN_POINT ( 'NONE',  ( 185.9653539490014111, -30.00000000000000000, 225.1241593668316625 ) ) ;
#9769 = DIRECTION ( 'NONE',  ( 0.6368676505102707219, 0.000000000000000000, 0.7709731485165535192 ) ) ;
#9770 = AXIS2_PLACEMENT_3D ( 'NONE', #9085, #7954, #10953 ) ;
#9771 = CARTESIAN_POINT ( 'NONE',  ( -242.1181102627692496, -6.423496681611010395, 10.13942498698713202 ) ) ;
#9772 = CARTESIAN_POINT ( 'NONE',  ( 150.6801963096165764, -19.40000000000000213, 241.8445669022807181 ) ) ;
#9773 = ITEM_DEFINED_TRANSFORMATION ( 'NONE', 'NONE', #9733,  #805 ) ;
#9774 = EDGE_LOOP ( 'NONE', ( #8122, #7158 ) ) ;
#9775 = CARTESIAN_POINT ( 'NONE',  ( -229.7675512415720789, 6.095529345594511206, 10.33836669620079185 ) ) ;
#9776 = AXIS2_PLACEMENT_3D ( 'NONE', #4265, #3124, #10394 ) ;
#9777 = ORIENTED_EDGE ( 'NONE', *, *, #2228, .T. ) ;
#9778 = ADVANCED_FACE ( 'NONE', ( #8250 ), #6440, .F. ) ;
#9779 = VECTOR ( 'NONE', #6522, 1000.000000000000000 ) ;
#9780 = EDGE_LOOP ( 'NONE', ( #8741, #8143 ) ) ;
#9781 = CARTESIAN_POINT ( 'NONE',  ( -248.7201528609607237, -10.06060527426557272, -6.070293049022396303 ) ) ;
#9782 = ORIENTED_EDGE ( 'NONE', *, *, #6486, .T. ) ;
#9783 = CARTESIAN_POINT ( 'NONE',  ( -226.7975291067479588, 20.55460285112940610, -130.9697226053176564 ) ) ;
#9784 = DIRECTION ( 'NONE',  ( -0.000000000000000000, -1.000000000000000000, 0.000000000000000000 ) ) ;
#9785 = DIRECTION ( 'NONE',  ( 0.6368676505102689456, 0.000000000000000000, 0.7709731485165549625 ) ) ;
#9786 = DIRECTION ( 'NONE',  ( 1.000000000000000000, 0.000000000000000000, 0.000000000000000000 ) ) ;
#9787 = AXIS2_PLACEMENT_3D ( 'NONE', #1802, #2909, #10060 ) ;
#9788 = CARTESIAN_POINT ( 'NONE',  ( -240.4621951198816987, 3.755930367962047711, 11.39707303937045602 ) ) ;
#9789 = EDGE_CURVE ( 'NONE', #10014, #11582, #422, .T. ) ;
#9790 = AXIS2_PLACEMENT_3D ( 'NONE', #6940, #868, #1868 ) ;
#9791 = DIRECTION ( 'NONE',  ( 0.6368676505102716101, 0.000000000000000000, 0.7709731485165527420 ) ) ;
#9792 = DIRECTION ( 'NONE',  ( -0.7660444431189726844, 0.000000000000000000, -0.6427876096865458022 ) ) ;
#9793 = CARTESIAN_POINT ( 'NONE',  ( 185.9653539490014111, -29.00000000000000000, 225.1241593668316625 ) ) ;
#9794 = AXIS2_PLACEMENT_3D ( 'NONE', #6916, #4767, #6974 ) ;
#9795 = CARTESIAN_POINT ( 'NONE',  ( -249.5826926912396573, 10.95569487812031184, -4.257357224325097000 ) ) ;
#9796 = CARTESIAN_POINT ( 'NONE',  ( -241.2266029203705102, -5.216955500352149500, -10.80672559041613212 ) ) ;
#9797 = DIRECTION ( 'NONE',  ( 0.000000000000000000, 1.000000000000000000, 0.000000000000000000 ) ) ;
#9798 = ORIENTED_EDGE ( 'NONE', *, *, #6555, .T. ) ;
#9799 = ORIENTED_EDGE ( 'NONE', *, *, #10671, .F. ) ;
#9800 = ORIENTED_EDGE ( 'NONE', *, *, #9154, .T. ) ;
#9801 = CARTESIAN_POINT ( 'NONE',  ( -122.2593324768321992, 30.00000000000000000, 174.7755348299905052 ) ) ;
#9802 = DIRECTION ( 'NONE',  ( 0.000000000000000000, 0.000000000000000000, -1.000000000000000000 ) ) ;
#9803 = EDGE_CURVE ( 'NONE', #779, #9649, #5798, .T. ) ;
#9804 = CARTESIAN_POINT ( 'NONE',  ( -172.3268284091859925, 20.79694577633260621, -196.4640694359954978 ) ) ;
#9805 = EDGE_CURVE ( 'NONE', #4466, #8628, #57, .T. ) ;
#9806 = CARTESIAN_POINT ( 'NONE',  ( 71.82423009839129691, 19.40000000000000213, -202.4354503650404808 ) ) ;
#9807 = DIRECTION ( 'NONE',  ( -0.8660254037844345998, 0.000000000000000000, -0.5000000000000071054 ) ) ;
#9808 = DIRECTION ( 'NONE',  ( -0.000000000000000000, 1.000000000000000000, 0.000000000000000000 ) ) ;
#9809 = CARTESIAN_POINT ( 'NONE',  ( 240.1760274753961824, 2.306688218039924188, -2.632364499241238054 ) ) ;
#9810 = PRESENTATION_LAYER_ASSIGNMENT (  '', '', ( #2366 ) ) ;
#9811 = ORIENTED_EDGE ( 'NONE', *, *, #5009, .F. ) ;
#9812 = AXIS2_PLACEMENT_3D ( 'NONE', #11587, #11451, #8648 ) ;
#9813 = EDGE_LOOP ( 'NONE', ( #9097, #12834 ) ) ;
#9814 = EDGE_CURVE ( 'NONE', #5691, #5106, #9623, .T. ) ;
#9815 = CARTESIAN_POINT ( 'NONE',  ( -238.7910754925967467, -0.6701662151381194699, 11.98127733947200646 ) ) ;
#9816 = EDGE_LOOP ( 'NONE', ( #44, #12383, #1364, #733 ) ) ;
#9817 = ORIENTED_EDGE ( 'NONE', *, *, #4554, .T. ) ;
#9818 = CIRCLE ( 'NONE', #8130, 6.500000000000005329 ) ;
#9819 = CARTESIAN_POINT ( 'NONE',  ( 17.05322212017792793, 20.08915143297736705, 260.1353576186482428 ) ) ;
#9820 = ORIENTED_EDGE ( 'NONE', *, *, #1992, .T. ) ;
#9821 = DIRECTION ( 'NONE',  ( 1.000000000000000000, 0.000000000000000000, 0.000000000000000000 ) ) ;
#9822 = CARTESIAN_POINT ( 'NONE',  ( -229.9928407511759474, -11.86219540972909847, 1.851581510365113648 ) ) ;
#9823 =( REPRESENTATION_RELATIONSHIP ('NONE','NONE', #12019, #182 ) REPRESENTATION_RELATIONSHIP_WITH_TRANSFORMATION ( #3499 )SHAPE_REPRESENTATION_RELATIONSHIP( ) );
#9824 = DIRECTION ( 'NONE',  ( 0.4503334343941690632, -0.7071067811865280328, 0.5451603414288133109 ) ) ;
#9825 = EDGE_CURVE ( 'NONE', #12286, #6909, #473, .T. ) ;
#9826 = LINE ( 'NONE', #5898, #7124 ) ;
#9827 = SHAPE_REPRESENTATION_RELATIONSHIP ( 'NONE' , 'NONE' ,  #11596, #10488 ) ;
#9828 = SURFACE_STYLE_FILL_AREA ( #4819 ) ;
#9829 = ORIENTED_EDGE ( 'NONE', *, *, #7034, .F. ) ;
#9830 = DIRECTION ( 'NONE',  ( -0.000000000000000000, -1.000000000000000000, 0.000000000000000000 ) ) ;
#9831 = ORIENTED_EDGE ( 'NONE', *, *, #5061, .F. ) ;
#9832 = CARTESIAN_POINT ( 'NONE',  ( -243.1949234309863641, 7.480730381643192928, -9.061063658798671483 ) ) ;
#9833 = VERTEX_POINT ( 'NONE', #4423 ) ;
#9834 = AXIS2_PLACEMENT_3D ( 'NONE', #9173, #3029, #3969 ) ;
#9835 = AXIS2_PLACEMENT_3D ( 'NONE', #5101, #5034, #11235 ) ;
#9836 = LINE ( 'NONE', #2633, #10888 ) ;
#9837 = CARTESIAN_POINT ( 'NONE',  ( -0.000000000000000000, -3.061616997868385015E-14, 0.000000000000000000 ) ) ;
#9838 = DIRECTION ( 'NONE',  ( -0.000000000000000000, -1.000000000000000000, 0.000000000000000000 ) ) ;
#9839 = AXIS2_PLACEMENT_3D ( 'NONE', #7198, #2197, #2259 ) ;
#9840 = CARTESIAN_POINT ( 'NONE',  ( -229.9694381604553541, 11.13630876764823263, -3.767427992309325457 ) ) ;
#9841 = CARTESIAN_POINT ( 'NONE',  ( -225.7689075324038583, 20.08915143297736705, 130.3442252640560639 ) ) ;
#9842 = PRODUCT_DEFINITION_SHAPE ( 'NONE', 'NONE',  #13154 ) ;
#9843 = CARTESIAN_POINT ( 'NONE',  ( -243.0412680530902207, -7.360923487768348927, 9.480357590559799874 ) ) ;
#9844 = VECTOR ( 'NONE', #11491, 1000.000000000000227 ) ;
#9845 = CARTESIAN_POINT ( 'NONE',  ( -239.4443750793461447, 1.773851997849018813, -11.86816533234759063 ) ) ;
#9846 = ITEM_DEFINED_TRANSFORMATION ( 'NONE', 'NONE', #2917,  #805 ) ;
#9847 = ORIENTED_EDGE ( 'NONE', *, *, #1571, .F. ) ;
#9848 = VECTOR ( 'NONE', #1310, 1000.000000000000000 ) ;
#9849 = DIRECTION ( 'NONE',  ( 0.000000000000000000, 0.000000000000000000, -1.000000000000000000 ) ) ;
#9850 = ORIENTED_EDGE ( 'NONE', *, *, #12261, .T. ) ;
#9851 = VERTEX_POINT ( 'NONE', #8508 ) ;
#9852 = CARTESIAN_POINT ( 'NONE',  ( -249.5485775756386033, -10.89766932192311621, -4.396091616435120919 ) ) ;
#9853 = ORIENTED_EDGE ( 'NONE', *, *, #6198, .F. ) ;
#9854 = CIRCLE ( 'NONE', #10921, 5.100000000000000533 ) ;
#9855 = CARTESIAN_POINT ( 'NONE',  ( -172.6991790963936921, 20.55460285138878618, 196.8887528212225106 ) ) ;
#9856 = DIRECTION ( 'NONE',  ( 0.000000000000000000, 0.000000000000000000, 1.000000000000000000 ) ) ;
#9857 = DIRECTION ( 'NONE',  ( 1.000000000000000000, 0.000000000000000000, 0.000000000000000000 ) ) ;
#9858 = AXIS2_PLACEMENT_3D ( 'NONE', #12530, #2526, #4391 ) ;
#9859 = CONICAL_SURFACE ( 'NONE', #5823, 5.500000000000005329, 0.7853981633974461696 ) ;
#9860 = CARTESIAN_POINT ( 'NONE',  ( 222.0845275804282153, 0.000000000000000000, 0.000000000000000000 ) ) ;
#9861 = ADVANCED_FACE ( 'NONE', ( #12570 ), #8618, .F. ) ;
#9862 = DIRECTION ( 'NONE',  ( 1.000000000000000000, 0.000000000000000000, 0.000000000000000000 ) ) ;
#9863 = EDGE_CURVE ( 'NONE', #5331, #1614, #7714, .T. ) ;
#9864 = DIRECTION ( 'NONE',  ( 0.000000000000000000, 0.000000000000000000, 1.000000000000000000 ) ) ;
#9865 = CARTESIAN_POINT ( 'NONE',  ( 26.90145978217153910, -138.4705547276867321, -32.05991134143103949 ) ) ;
#9866 = AXIS2_PLACEMENT_3D ( 'NONE', #236, #8379, #12438 ) ;
#9867 = CARTESIAN_POINT ( 'NONE',  ( 229.9999970288534712, 3.499804753153490378, -0.2337124727541820546 ) ) ;
#9868 = AXIS2_PLACEMENT_3D ( 'NONE', #1465, #8539, #5529 ) ;
#9869 = CARTESIAN_POINT ( 'NONE',  ( -249.7048772684788105, 11.25744417597311475, 3.375279421353320597 ) ) ;
#9870 = DIRECTION ( 'NONE',  ( 0.000000000000000000, 0.000000000000000000, 1.000000000000000000 ) ) ;
#9871 = FACE_OUTER_BOUND ( 'NONE', #8807, .T. ) ;
#9872 = ORIENTED_EDGE ( 'NONE', *, *, #12541, .T. ) ;
#9873 = ORIENTED_EDGE ( 'NONE', *, *, #3273, .F. ) ;
#9874 = DIRECTION ( 'NONE',  ( 0.000000000000000000, 0.000000000000000000, 1.000000000000000000 ) ) ;
#9875 = CARTESIAN_POINT ( 'NONE',  ( 290.6841825403032544, -30.00000000000000000, 27.68945685411186730 ) ) ;
#9876 = PRODUCT_DEFINITION_SHAPE ( 'NONE', 'NONE',  #13063 ) ;
#9877 = CIRCLE ( 'NONE', #5848, 6.500000000000000000 ) ;
#9878 = AXIS2_PLACEMENT_3D ( 'NONE', #10329, #1206, #3455 ) ;
#9879 = CARTESIAN_POINT ( 'NONE',  ( 234.8993005733554185, 20.55460285121469610, -115.8123742911327838 ) ) ;
#9880 = DIRECTION ( 'NONE',  ( 0.000000000000000000, 0.000000000000000000, 1.000000000000000000 ) ) ;
#9881 = CARTESIAN_POINT ( 'NONE',  ( 0.000000000000000000, 0.000000000000000000, 0.000000000000000000 ) ) ;
#9882 = DIRECTION ( 'NONE',  ( 0.000000000000000000, 1.000000000000000000, 0.000000000000000000 ) ) ;
#9883 = DIRECTION ( 'NONE',  ( 0.000000000000000000, 1.000000000000000000, 0.000000000000000000 ) ) ;
#9884 = ORIENTED_EDGE ( 'NONE', *, *, #10554, .T. ) ;
#9885 = CIRCLE ( 'NONE', #6273, 5.100000000000003197 ) ;
#9886 = CARTESIAN_POINT ( 'NONE',  ( -239.7835669413218795, -2.057906908539555602, 11.82250766381889839 ) ) ;
#9887 = VERTEX_POINT ( 'NONE', #10568 ) ;
#9888 = EDGE_LOOP ( 'NONE', ( #8632, #9071, #4050, #625 ) ) ;
#9889 = EDGE_CURVE ( 'NONE', #6308, #6838, #5800, .T. ) ;
#9890 = EDGE_CURVE ( 'NONE', #7200, #4744, #5498, .T. ) ;
#9891 = DIRECTION ( 'NONE',  ( 0.000000000000000000, 1.000000000000000000, 0.000000000000000000 ) ) ;
#9892 = ORIENTED_EDGE ( 'NONE', *, *, #3516, .F. ) ;
#9893 = DIRECTION ( 'NONE',  ( 0.000000000000000000, 0.9998057603070481525, -0.01970892327970899874 ) ) ;
#9894 = PLANE ( 'NONE',  #1118 ) ;
#9895 = AXIS2_PLACEMENT_3D ( 'NONE', #7988, #11916, #3844 ) ;
#9896 = DIRECTION ( 'NONE',  ( -0.000000000000000000, -1.000000000000000000, 0.000000000000000000 ) ) ;
#9897 = FACE_OUTER_BOUND ( 'NONE', #8758, .T. ) ;
#9898 = ORIENTED_EDGE ( 'NONE', *, *, #8914, .F. ) ;
#9899 = DIRECTION ( 'NONE',  ( 8.659560562354913137E-17, -0.7071067811865489050, 0.7071067811865460184 ) ) ;
#9900 = ORIENTED_EDGE ( 'NONE', *, *, #4196, .T. ) ;
#9901 = CARTESIAN_POINT ( 'NONE',  ( -248.0831933713610056, 9.830508068705238856, -6.436117704883929314 ) ) ;
#9902 = VERTEX_POINT ( 'NONE', #3293 ) ;
#9903 = TOROIDAL_SURFACE ( 'NONE', #3934, 247.7999999999999829, 2.000000000000000000 ) ;
#9904 = EDGE_CURVE ( 'NONE', #690, #1431, #5381, .T. ) ;
#9905 = CIRCLE ( 'NONE', #4156, 249.0000000000000284 ) ;
#9906 = DIRECTION ( 'NONE',  ( -0.000000000000000000, -1.000000000000000000, 0.000000000000000000 ) ) ;
#9907 = CARTESIAN_POINT ( 'NONE',  ( 240.2816503055764485, 2.505215826442440896, 2.444791323487650825 ) ) ;
#9908 = CARTESIAN_POINT ( 'NONE',  ( -197.8197553893909912, 19.00000000000000000, 64.27553482999130097 ) ) ;
#9909 = CARTESIAN_POINT ( 'NONE',  ( -229.6996680450365034, 7.200459016985159977E-17, -11.75000000000000000 ) ) ;
#9910 = EDGE_CURVE ( 'NONE', #7179, #1904, #8382, .T. ) ;
#9911 = CARTESIAN_POINT ( 'NONE',  ( -243.9837273761031042, 20.08915143297736705, 91.83222442980193989 ) ) ;
#9912 = CARTESIAN_POINT ( 'NONE',  ( -242.3388033292662271, -6.664155344899789668, 9.979432606853753995 ) ) ;
#9913 = AXIS2_PLACEMENT_3D ( 'NONE', #2104, #3409, #2421 ) ;
#9914 = CARTESIAN_POINT ( 'NONE',  ( -238.9765878232742580, 1.145734735638040735, -11.94560817730083890 ) ) ;
#9915 = CONTEXT_DEPENDENT_SHAPE_REPRESENTATION ( #11627, #10321 ) ;
#9916 = ORIENTED_EDGE ( 'NONE', *, *, #1165, .F. ) ;
#9917 = CARTESIAN_POINT ( 'NONE',  ( -238.7452658386391420, -0.4192328095118098008, -11.74262570625762692 ) ) ;
#9918 = AXIS2_PLACEMENT_3D ( 'NONE', #6080, #10009, #8075 ) ;
#9919 = ORIENTED_EDGE ( 'NONE', *, *, #1708, .F. ) ;
#9920 = ORIENTED_EDGE ( 'NONE', *, *, #1742, .F. ) ;
#9921 = CARTESIAN_POINT ( 'NONE',  ( -0.000000000000000000, -22.00000000000000000, 0.000000000000000000 ) ) ;
#9922 = ORIENTED_EDGE ( 'NONE', *, *, #218, .F. ) ;
#9923 = CARTESIAN_POINT ( 'NONE',  ( 130.9697226058085846, 20.55460285117392516, 226.7975291051602937 ) ) ;
#9924 = CARTESIAN_POINT ( 'NONE',  ( -245.4297298671266674, 8.960803861242091273, -7.981710862854209054 ) ) ;
#9925 = CARTESIAN_POINT ( 'NONE',  ( -0.000000000000000000, -29.00000000000000000, 0.000000000000000000 ) ) ;
#9926 = DIRECTION ( 'NONE',  ( 1.000000000000000000, 0.000000000000000000, 0.000000000000000000 ) ) ;
#9927 = CARTESIAN_POINT ( 'NONE',  ( 229.9000000000000057, -4.447920636657316074, 2.686261716586446635 ) ) ;
#9928 = DIRECTION ( 'NONE',  ( -0.7071067811865512365, 0.000000000000000000, 0.7071067811865437980 ) ) ;
#9929 = CARTESIAN_POINT ( 'NONE',  ( 290.6841825403032544, -30.00000000000000000, 27.68945685411186730 ) ) ;
#9930 = CARTESIAN_POINT ( 'NONE',  ( -249.7634162175664301, 11.48172780046974850, -2.515098136597289979 ) ) ;
#9931 = CARTESIAN_POINT ( 'NONE',  ( -229.8080432352570313, -7.471644199020397004, -9.397490282286900865 ) ) ;
#9932 = ORIENTED_EDGE ( 'NONE', *, *, #3985, .F. ) ;
#9933 = ORIENTED_EDGE ( 'NONE', *, *, #4675, .T. ) ;
#9934 = EDGE_CURVE ( 'NONE', #12435, #11682, #5632, .T. ) ;
#9935 = DIRECTION ( 'NONE',  ( 1.000000000000000000, 0.000000000000000000, 0.000000000000000000 ) ) ;
#9936 = CYLINDRICAL_SURFACE ( 'NONE', #1140, 8.000000000000007105 ) ;
#9937 = CIRCLE ( 'NONE', #4191, 10.00000000000000888 ) ;
#9938 = CARTESIAN_POINT ( 'NONE',  ( 247.4557548102664839, 20.79694577621951979, -84.02568524171830688 ) ) ;
#9939 = DIRECTION ( 'NONE',  ( 0.000000000000000000, 1.000000000000000000, 0.000000000000000000 ) ) ;
#9940 = DIRECTION ( 'NONE',  ( -1.000000000000000000, 0.000000000000000000, -6.982962677686266711E-15 ) ) ;
#9941 = CARTESIAN_POINT ( 'NONE',  ( 240.0429366796199702, 2.111384149270551625, -2.791848677271159485 ) ) ;
#9942 = CONICAL_SURFACE ( 'NONE', #8256, 5.499999999999998224, 0.7853981633974461696 ) ;
#9943 = B_SPLINE_CURVE_WITH_KNOTS ( 'NONE', 3,
 ( #10209, #8358, #11149, #2145, #6223, #11417, #1016, #1152, #3270, #5142, #6092, #7087, #5212, #2020, #7352, #10410, #5071, #1286, #2274, #9286, #11350, #156, #4079, #8422, #2215, #12354, #4209, #1217, #6352, #8293, #5349, #10343, #9149, #3205 ),
 .UNSPECIFIED., .F., .F.,
 ( 4, 2, 2, 2, 2, 2, 2, 2, 2, 2, 2, 2, 2, 2, 2, 2, 4 ),
 ( 8.253566423007127763E-20, 0.0006839223821429840340, 0.001367844764285967851, 0.002051767146428951343, 0.002735689528571936136, 0.003419611910714920929, 0.004103534292857904421, 0.004787456675000889214, 0.005471379057143873140, 0.006155301439286857933, 0.006839223821429841858, 0.007523146203572825784, 0.008207068585715808842, 0.008890990967858792768, 0.009574913350001776693, 0.01025883573214476062, 0.01094275811428774454 ),
 .UNSPECIFIED. ) ;
#9944 = ORIENTED_EDGE ( 'NONE', *, *, #9889, .F. ) ;
#9945 = FACE_BOUND ( 'NONE', #9029, .T. ) ;
#9946 = CARTESIAN_POINT ( 'NONE',  ( 3.059167704270088292E-14, 0.000000000000000000, 249.7999999999999829 ) ) ;
#9947 = ORIENTED_EDGE ( 'NONE', *, *, #4772, .T. ) ;
#9948 = ORIENTED_EDGE ( 'NONE', *, *, #5467, .T. ) ;
#9949 = ADVANCED_FACE ( 'NONE', ( #2814 ), #2598, .T. ) ;
#9950 = PRODUCT_DEFINITION_CONTEXT ( 'detailed design', #472, 'design' ) ;
#9951 = DIRECTION ( 'NONE',  ( 0.000000000000000000, 0.000000000000000000, 1.000000000000000000 ) ) ;
#9952 = ORIENTED_EDGE ( 'NONE', *, *, #1735, .F. ) ;
#9953 = PRODUCT_DEFINITION_SHAPE ( 'NONE', 'NONE',  #13158 ) ;
#9954 = CARTESIAN_POINT ( 'NONE',  ( 221.6213872890270977, -19.00000000000000000, -190.2057062658400923 ) ) ;
#9955 =( GEOMETRIC_REPRESENTATION_CONTEXT ( 3 ) GLOBAL_UNCERTAINTY_ASSIGNED_CONTEXT ( ( #8428 ) ) GLOBAL_UNIT_ASSIGNED_CONTEXT ( ( #707, #9959, #13027 ) ) REPRESENTATION_CONTEXT ( 'NONE', 'WORKASPACE' ) );
#9956 =( REPRESENTATION_RELATIONSHIP ('NONE','NONE', #12019, #5191 ) REPRESENTATION_RELATIONSHIP_WITH_TRANSFORMATION ( #4448 )SHAPE_REPRESENTATION_RELATIONSHIP( ) );
#9957 = DIRECTION ( 'NONE',  ( -0.000000000000000000, -1.000000000000000000, 0.000000000000000000 ) ) ;
#9958 = CARTESIAN_POINT ( 'NONE',  ( 0.000000000000000000, 23.50000000000000000, -246.0000000000000000 ) ) ;
#9959 =( NAMED_UNIT ( * ) PLANE_ANGLE_UNIT ( ) SI_UNIT ( $, .RADIAN. ) );
#9960 = DIRECTION ( 'NONE',  ( -0.6368676505102706109, 0.000000000000000000, -0.7709731485165535192 ) ) ;
#9961 = EDGE_CURVE ( 'NONE', #12935, #10237, #10061, .T. ) ;
#9962 = EDGE_CURVE ( 'NONE', #6293, #1635, #12406, .T. ) ;
#9963 = ORIENTED_EDGE ( 'NONE', *, *, #2134, .T. ) ;
#9964 = LINE ( 'NONE', #9098, #10723 ) ;
#9966 = VERTEX_POINT ( 'NONE', #6772 ) ;
#9965 = AXIS2_PLACEMENT_3D ( 'NONE', #7346, #3128, #9280 ) ;
#9967 = DIRECTION ( 'NONE',  ( 0.000000000000000000, -1.000000000000000000, 0.000000000000000000 ) ) ;
#9968 = ORIENTED_EDGE ( 'NONE', *, *, #1420, .F. ) ;
#9969 = DIRECTION ( 'NONE',  ( 0.000000000000000000, 0.000000000000000000, 1.000000000000000000 ) ) ;
#9970 = CARTESIAN_POINT ( 'NONE',  ( -161.8917567597108587, 0.000000000000000000, -195.9813743529078636 ) ) ;
#9971 = CARTESIAN_POINT ( 'NONE',  ( -27.68945685411286561, -30.00000000000000000, 290.6841825403027997 ) ) ;
#9972 = AXIS2_PLACEMENT_3D ( 'NONE', #357, #5479, #1221 ) ;
#9973 = VECTOR ( 'NONE', #10023, 1000.000000000000114 ) ;
#9974 = AXIS2_PLACEMENT_3D ( 'NONE', #11488, #28, #2219 ) ;
#9975 = CARTESIAN_POINT ( 'NONE',  ( -229.7432275410588716, 4.515244320528268851, -10.86800257939080971 ) ) ;
#9976 = AXIS2_PLACEMENT_3D ( 'NONE', #12390, #3244, #7132 ) ;
#9977 = CARTESIAN_POINT ( 'NONE',  ( -34.02434144668606564, 20.08915143297736705, 258.4638482596384961 ) ) ;
#9978 = AXIS2_PLACEMENT_3D ( 'NONE', #5625, #1621, #6633 ) ;
#9979 = CARTESIAN_POINT ( 'NONE',  ( -243.6755871756507759, -7.880721788829696095, 9.049489450807712387 ) ) ;
#9980 = ADVANCED_FACE ( 'NONE', ( #7819, #5696 ), #9894, .F. ) ;
#9981 = ADVANCED_FACE ( 'NONE', ( #635 ), #12447, .T. ) ;
#9982 = CARTESIAN_POINT ( 'NONE',  ( -238.8648708987263376, 0.8933728665143385594, -11.96676141167906948 ) ) ;
#9983 = UNCERTAINTY_MEASURE_WITH_UNIT (LENGTH_MEASURE( 1.000000000000000082E-05 ), #10967, 'distance_accuracy_value', 'NONE');
#9984 = EDGE_LOOP ( 'NONE', ( #3750, #11214, #2790, #2217 ) ) ;
#9985 = CARTESIAN_POINT ( 'NONE',  ( -239.0190678775036304, -1.196910341722188242, -11.68891451112129864 ) ) ;
#9986 = ORIENTED_EDGE ( 'NONE', *, *, #2081, .T. ) ;
#9987 = EDGE_CURVE ( 'NONE', #1760, #5790, #8573, .T. ) ;
#9988 = VERTEX_POINT ( 'NONE', #4140 ) ;
#9989 = AXIS2_PLACEMENT_3D ( 'NONE', #10249, #3178, #11324 ) ;
#9990 = CARTESIAN_POINT ( 'NONE',  ( -249.7838850256695764, -11.60404975226508739, -1.846229155068394467 ) ) ;
#9991 = VERTEX_POINT ( 'NONE', #8221 ) ;
#9992 = CARTESIAN_POINT ( 'NONE',  ( -159.4136521825795114, 20.55460285040709678, 207.7919029861446916 ) ) ;
#9993 = EDGE_CURVE ( 'NONE', #5790, #1760, #4407, .T. ) ;
#9994 = VECTOR ( 'NONE', #12023, 1000.000000000000000 ) ;
#9995 = CARTESIAN_POINT ( 'NONE',  ( 150.6801963096165764, -19.40000000000000213, 241.8445669022807181 ) ) ;
#9996 = CARTESIAN_POINT ( 'NONE',  ( -247.9656915563521977, -9.808762669708828597, -6.469331566110803955 ) ) ;
#9997 = CARTESIAN_POINT ( 'NONE',  ( -243.9120028876667163, 8.059256684570714313, 8.893843983381984231 ) ) ;
#9998 = EDGE_CURVE ( 'NONE', #5893, #5922, #11005, .T. ) ;
#9999 = FILL_AREA_STYLE_COLOUR ( '', #4567 ) ;
#10000 = DIRECTION ( 'NONE',  ( 0.5351817705578594264, 0.5538822189107471816, -0.6378047977532482760 ) ) ;
#10001 = CARTESIAN_POINT ( 'NONE',  ( -229.9923139574567585, -11.59881862766272320, 1.917681925180096281 ) ) ;
#10002 = ITEM_DEFINED_TRANSFORMATION ( 'NONE', 'NONE', #9385,  #805 ) ;
#10003 =( REPRESENTATION_RELATIONSHIP ('NONE','NONE', #12019, #182 ) REPRESENTATION_RELATIONSHIP_WITH_TRANSFORMATION ( #8452 )SHAPE_REPRESENTATION_RELATIONSHIP( ) );
#10004 = DIRECTION ( 'NONE',  ( -1.000000000000000000, 0.000000000000000000, 0.000000000000000000 ) ) ;
#10005 = ORIENTED_EDGE ( 'NONE', *, *, #8882, .T. ) ;
#10006 = EDGE_LOOP ( 'NONE', ( #10917, #65 ) ) ;
#10007 = AXIS2_PLACEMENT_3D ( 'NONE', #10822, #12825, #11836 ) ;
#10008 = CARTESIAN_POINT ( 'NONE',  ( -17.05314194195814892, 20.08915143288246696, 260.5542428355875018 ) ) ;
#10009 = DIRECTION ( 'NONE',  ( 0.000000000000000000, 1.000000000000000000, 0.000000000000000000 ) ) ;
#10010 = CARTESIAN_POINT ( 'NONE',  ( 260.7745447061710138, 20.79694577634651509, -17.06760680878044667 ) ) ;
#10011 = DIRECTION ( 'NONE',  ( 0.000000000000000000, 0.000000000000000000, 1.000000000000000000 ) ) ;
#10012 = DIRECTION ( 'NONE',  ( -0.5735764363510391650, 0.000000000000000000, -0.8191520442889966835 ) ) ;
#10013 = CARTESIAN_POINT ( 'NONE',  ( -242.9139448622711654, -7.229284208925894184, 9.262738308019747180 ) ) ;
#10014 = VERTEX_POINT ( 'NONE', #11141 ) ;
#10015 =( REPRESENTATION_RELATIONSHIP ('NONE','NONE', #12019, #182 ) REPRESENTATION_RELATIONSHIP_WITH_TRANSFORMATION ( #1012 )SHAPE_REPRESENTATION_RELATIONSHIP( ) );
#10016 = LINE ( 'NONE', #3845, #9994 ) ;
#10017 = AXIS2_PLACEMENT_3D ( 'NONE', #3393, #8665, #8478 ) ;
#10018 = CARTESIAN_POINT ( 'NONE',  ( -239.6279820725406751, -1.937806661696064969, 11.84250614284618131 ) ) ;
#10019 = EDGE_LOOP ( 'NONE', ( #5435, #9798, #9853, #8329 ) ) ;
#10020 = ORIENTED_EDGE ( 'NONE', *, *, #6529, .F. ) ;
#10021 = DIRECTION ( 'NONE',  ( -0.6368676505102707219, 0.000000000000000000, -0.7709731485165536302 ) ) ;
#10022 = CARTESIAN_POINT ( 'NONE',  ( 135.8846079354933352, -28.60000000000000142, -256.1940150085812888 ) ) ;
#10023 = DIRECTION ( 'NONE',  ( 8.659560562354913137E-17, -0.7071067811865489050, 0.7071067811865460184 ) ) ;
#10024 = CARTESIAN_POINT ( 'NONE',  ( 83.95474316029249451, 20.08915143279689630, 247.2466869562504996 ) ) ;
#10025 = ITEM_DEFINED_TRANSFORMATION ( 'NONE', 'NONE', #7042,  #805 ) ;
#10026 = CARTESIAN_POINT ( 'NONE',  ( -239.4378968521887998, -1.767436680809186145, -11.86912576102403705 ) ) ;
#10027 = SHAPE_REPRESENTATION_RELATIONSHIP ( 'NONE' , 'NONE' ,  #5191, #13034 ) ;
#10028 = CARTESIAN_POINT ( 'NONE',  ( 0.000000000000000000, 3.327561323230765034, 238.4705882352940307 ) ) ;
#10029 = ADVANCED_FACE ( 'NONE', ( #1877 ), #948, .F. ) ;
#10030 = EDGE_CURVE ( 'NONE', #5691, #10752, #7504, .T. ) ;
#10031 = VERTEX_POINT ( 'NONE', #8080 ) ;
#10032 = CARTESIAN_POINT ( 'NONE',  ( -239.1821278489683209, -1.453791005755859400, 11.65971745006329385 ) ) ;
#10034 = VERTEX_POINT ( 'NONE', #3999 ) ;
#10033 = VECTOR ( 'NONE', #10904, 1000.000000000000114 ) ;
#10035 = EDGE_LOOP ( 'NONE', ( #8241, #7510 ) ) ;
#10036 = AXIS2_PLACEMENT_3D ( 'NONE', #10645, #7774, #12906 ) ;
#10037 = VECTOR ( 'NONE', #9899, 1000.000000000000114 ) ;
#10038 = ADVANCED_FACE ( 'NONE', ( #878 ), #8014, .F. ) ;
#10039 = CARTESIAN_POINT ( 'NONE',  ( -0.000000000000000000, -29.00000000000000000, 0.000000000000000000 ) ) ;
#10040 = DIRECTION ( 'NONE',  ( 0.000000000000000000, 1.000000000000000000, 0.000000000000000000 ) ) ;
#10041 = CARTESIAN_POINT ( 'NONE',  ( 238.9791647118827029, 0.1781744854528612421, 3.496576182270254574 ) ) ;
#10042 = CARTESIAN_POINT ( 'NONE',  ( 122.2593324768346008, 30.00000000000000000, 168.2755348299889988 ) ) ;
#10043 = DIRECTION ( 'NONE',  ( 1.000000000000000000, 0.000000000000000000, 0.000000000000000000 ) ) ;
#10044 = CARTESIAN_POINT ( 'NONE',  ( -244.2463344796078957, -8.285434989118469318, 8.680536403647563404 ) ) ;
#10045 = CARTESIAN_POINT ( 'NONE',  ( -196.1676464792605259, 20.79694577634646535, -172.0303573358525000 ) ) ;
#10046 = VERTEX_POINT ( 'NONE', #6017 ) ;
#10047 = DIRECTION ( 'NONE',  ( -0.000000000000000000, 0.4828344519120574274, -0.8757116489157735773 ) ) ;
#10048 = VECTOR ( 'NONE', #7045, 1000.000000000000114 ) ;
#10049 = ORIENTED_EDGE ( 'NONE', *, *, #8104, .F. ) ;
#10050 = VERTEX_POINT ( 'NONE', #2995 ) ;
#10051 = DIRECTION ( 'NONE',  ( 0.000000000000000000, 0.000000000000000000, -1.000000000000000000 ) ) ;
#10052 = VERTEX_POINT ( 'NONE', #7078 ) ;
#10053 = ADVANCED_FACE ( 'NONE', ( #6084 ), #10134, .F. ) ;
#10054 = CONICAL_SURFACE ( 'NONE', #11968, 305.0000000000000000, 0.7853981633974758125 ) ;
#10055 = CARTESIAN_POINT ( 'NONE',  ( -1.009183486025028462E-12, 20.55460285106647689, 261.3381329044966606 ) ) ;
#10056 = ADVANCED_FACE ( 'NONE', ( #3196 ), #1143, .T. ) ;
#10057 = CARTESIAN_POINT ( 'NONE',  ( 71.82423009839129691, 30.00000000000000000, -203.8354503650404865 ) ) ;
#10058 = CARTESIAN_POINT ( 'NONE',  ( 233.5975020798683204, 0.000000000000000000, 0.000000000000000000 ) ) ;
#10059 = TOROIDAL_SURFACE ( 'NONE', #70, 250.0000000000000000, 10.00000000000000000 ) ;
#10060 = DIRECTION ( 'NONE',  ( 0.000000000000000000, 0.000000000000000000, 1.000000000000000000 ) ) ;
#10061 = CIRCLE ( 'NONE', #484, 5.100000000000003197 ) ;
#10062 = CARTESIAN_POINT ( 'NONE',  ( -242.3038136696739002, 6.626013037278306150, 10.00479684789553048 ) ) ;
#10063 = SURFACE_SIDE_STYLE ('',( #996 ) ) ;
#10064 = DIRECTION ( 'NONE',  ( 0.8191520442889986819, 0.000000000000000000, -0.5735764363510362784 ) ) ;
#10065 = CARTESIAN_POINT ( 'NONE',  ( -229.8697759883668539, -8.858708711567949479, 7.758056923234300406 ) ) ;
#10066 = CARTESIAN_POINT ( 'NONE',  ( -229.7550362174501686, -5.611521452489740547, -10.61368970446696380 ) ) ;
#10067 = ORIENTED_EDGE ( 'NONE', *, *, #2878, .F. ) ;
#10068 = VERTEX_POINT ( 'NONE', #5203 ) ;
#10069 = CARTESIAN_POINT ( 'NONE',  ( -23.54981712579610331, -30.00000000000000000, 295.6955080056604288 ) ) ;
#10070 = EDGE_CURVE ( 'NONE', #5758, #7894, #1337, .T. ) ;
#10071 = CARTESIAN_POINT ( 'NONE',  ( 0.000000000000000000, 1.848645179567965036, 0.000000000000000000 ) ) ;
#10072 = DIRECTION ( 'NONE',  ( 0.6368676505102716101, 0.000000000000000000, 0.7709731485165527420 ) ) ;
#10073 = CIRCLE ( 'NONE', #293, 5.500000000000005329 ) ;
#10074 = DIRECTION ( 'NONE',  ( 0.000000000000000000, -1.000000000000000000, 0.000000000000000000 ) ) ;
#10075 = AXIS2_PLACEMENT_3D ( 'NONE', #1442, #9758, #573 ) ;
#10076 = DIRECTION ( 'NONE',  ( -0.000000000000000000, -1.000000000000000000, 0.000000000000000000 ) ) ;
#10077 = DIRECTION ( 'NONE',  ( 0.6427876096865481337, 0.000000000000000000, -0.7660444431189706860 ) ) ;
#10078 = AXIS2_PLACEMENT_3D ( 'NONE', #7420, #7556, #3544 ) ;
#10079 = CARTESIAN_POINT ( 'NONE',  ( -243.9217790761123581, -8.053804826441991693, 8.555499786857474476 ) ) ;
#10080 = ITEM_DEFINED_TRANSFORMATION ( 'NONE', 'NONE', #10388,  #805 ) ;
#10081 =( REPRESENTATION_RELATIONSHIP ('NONE','NONE', #12019, #182 ) REPRESENTATION_RELATIONSHIP_WITH_TRANSFORMATION ( #54 )SHAPE_REPRESENTATION_RELATIONSHIP( ) );
#10082 = VERTEX_POINT ( 'NONE', #1589 ) ;
#10083 = CARTESIAN_POINT ( 'NONE',  ( 192.8974817588416784, -22.00000000000000000, -159.3442861576696998 ) ) ;
#10084 = DIRECTION ( 'NONE',  ( 0.000000000000000000, 0.000000000000000000, 1.000000000000000000 ) ) ;
#10085 = EDGE_LOOP ( 'NONE', ( #10755, #7007 ) ) ;
#10086 = ORIENTED_EDGE ( 'NONE', *, *, #253, .T. ) ;
#10087 = CARTESIAN_POINT ( 'NONE',  ( -5.000000000000000000, 9.797174393178815797E-16, 242.0000000000000000 ) ) ;
#10088 = CYLINDRICAL_SURFACE ( 'NONE', #12946, 250.1999999999999602 ) ;
#10089 = CARTESIAN_POINT ( 'NONE',  ( -248.3468897629254286, 9.892776367310945673, 6.340645126600181314 ) ) ;
#10090 = CARTESIAN_POINT ( 'NONE',  ( 172.1812796676979929, 20.08915143304314910, -196.2980642831070099 ) ) ;
#10091 = CARTESIAN_POINT ( 'NONE',  ( -239.0379403834560605, -1.251320448579115618, -11.93458158033107175 ) ) ;
#10092 = CARTESIAN_POINT ( 'NONE',  ( -242.3262939448890450, 6.637532586066957840, 9.695808799222838559 ) ) ;
#10093 = ORIENTED_EDGE ( 'NONE', *, *, #6394, .T. ) ;
#10094 = DIRECTION ( 'NONE',  ( -0.4503334343941556295, 0.7071067811865489050, -0.5451603414287969906 ) ) ;
#10095 = ORIENTED_EDGE ( 'NONE', *, *, #12961, .T. ) ;
#10096 = CARTESIAN_POINT ( 'NONE',  ( -239.0839813628342370, 1.310043309152621571, 11.67696021899406134 ) ) ;
#10097 = VERTEX_POINT ( 'NONE', #10648 ) ;
#10098 = ADVANCED_FACE ( 'NONE', ( #1518 ), #13036, .F. ) ;
#10099 = EDGE_CURVE ( 'NONE', #7354, #6957, #8367, .T. ) ;
#10100 = CIRCLE ( 'NONE', #5201, 6.500000000000000888 ) ;
#10101 = DIRECTION ( 'NONE',  ( 0.000000000000000000, 0.9998057603070481525, -0.01970892327970899874 ) ) ;
#10102 = CARTESIAN_POINT ( 'NONE',  ( -182.4625818711933221, -19.00000000000000000, -220.8838070499919013 ) ) ;
#10103 = CYLINDRICAL_SURFACE ( 'NONE', #4024, 250.1999999999999602 ) ;
#10104 =( REPRESENTATION_RELATIONSHIP ('NONE','NONE', #12019, #5191 ) REPRESENTATION_RELATIONSHIP_WITH_TRANSFORMATION ( #2127 )SHAPE_REPRESENTATION_RELATIONSHIP( ) );
#10105 = FACE_OUTER_BOUND ( 'NONE', #12851, .T. ) ;
#10106 = LINE ( 'NONE', #12045, #10526 ) ;
#10107 = FACE_OUTER_BOUND ( 'NONE', #5249, .T. ) ;
#10108 = CARTESIAN_POINT ( 'NONE',  ( -239.0548353904412124, 1.279873199972036968, -11.93155240843870146 ) ) ;
#10109 = ORIENTED_EDGE ( 'NONE', *, *, #5154, .F. ) ;
#10110 = CARTESIAN_POINT ( 'NONE',  ( -238.7109915777814138, -2.671037648644427152E-08, -11.74999999995326050 ) ) ;
#10111 = MECHANICAL_DESIGN_GEOMETRIC_PRESENTATION_REPRESENTATION (  '', ( #3288 ), #6290 ) ;
#10112 = ORIENTED_EDGE ( 'NONE', *, *, #4901, .T. ) ;
#10113 = CARTESIAN_POINT ( 'NONE',  ( -247.0695545832770961, -9.592608482351387522, -7.209588857372366988 ) ) ;
#10114 = CARTESIAN_POINT ( 'NONE',  ( -249.7006323030246051, -11.24927497773904861, 3.394647654957348326 ) ) ;
#10115 = ORIENTED_EDGE ( 'NONE', *, *, #2273, .F. ) ;
#10116 = EDGE_CURVE ( 'NONE', #3851, #167, #9278, .T. ) ;
#10117 = CARTESIAN_POINT ( 'NONE',  ( 130.6873781525580114, 20.79694577610125705, 226.3083638772055224 ) ) ;
#10118 = CARTESIAN_POINT ( 'NONE',  ( -246.8633775079653390, 9.531357830558160771, -7.291317144092957392 ) ) ;
#10119 = CARTESIAN_POINT ( 'NONE',  ( -240.0143494547118337, 2.418590315959113113, 11.50416929268522281 ) ) ;
#10120 = CARTESIAN_POINT ( 'NONE',  ( -246.6923348785073244, -9.470909649843260780, -6.954450552458404822 ) ) ;
#10121 = AXIS2_PLACEMENT_3D ( 'NONE', #3612, #7618, #9677 ) ;
#10122 = CONICAL_SURFACE ( 'NONE', #8218, 248.7999999999999829, 0.7853981633974348453 ) ;
#10123 = CARTESIAN_POINT ( 'NONE',  ( -249.8000249158748716, 12.00052859681964890, -0.5791969794655120740 ) ) ;
#10124 = DIRECTION ( 'NONE',  ( 0.6427876096865481337, 0.000000000000000000, -0.7660444431189706860 ) ) ;
#10125 = EDGE_CURVE ( 'NONE', #497, #1017, #12777, .T. ) ;
#10126 = DIRECTION ( 'NONE',  ( -0.6368676505102706109, 0.000000000000000000, -0.7709731485165535192 ) ) ;
#10127 = ADVANCED_FACE ( 'NONE', ( #7344 ), #272, .F. ) ;
#10128 = CARTESIAN_POINT ( 'NONE',  ( 122.2593324768346008, 29.00000000000000000, 173.7755348299889988 ) ) ;
#10129 = ORIENTED_EDGE ( 'NONE', *, *, #816, .T. ) ;
#10130 = EDGE_LOOP ( 'NONE', ( #4545, #10625 ) ) ;
#10131 = CARTESIAN_POINT ( 'NONE',  ( -196.2980642832790181, 20.08915143307791951, 172.1812796672794832 ) ) ;
#10132 = CARTESIAN_POINT ( 'NONE',  ( 0.000000000000000000, 29.00000000000000000, 0.000000000000000000 ) ) ;
#10133 = DIRECTION ( 'NONE',  ( 1.000000000000000000, 0.000000000000000000, 0.000000000000000000 ) ) ;
#10134 = CYLINDRICAL_SURFACE ( 'NONE', #6023, 5.500000000000005329 ) ;
#10135 = LINE ( 'NONE', #2210, #12414 ) ;
#10136 = DIRECTION ( 'NONE',  ( -0.07256543843575807839, 0.5538822189107472926, 0.8294267566935212832 ) ) ;
#10137 = LINE ( 'NONE', #1011, #8006 ) ;
#10138 = CONTEXT_DEPENDENT_SHAPE_REPRESENTATION ( #2515, #8046 ) ;
#10139 = EDGE_CURVE ( 'NONE', #5992, #11915, #8283, .T. ) ;
#10140 = ORIENTED_EDGE ( 'NONE', *, *, #11632, .F. ) ;
#10141 = FACE_BOUND ( 'NONE', #10085, .T. ) ;
#10142 = CARTESIAN_POINT ( 'NONE',  ( -290.6841825403030839, -30.00000000000000000, -27.68945685411394919 ) ) ;
#10143 = ORIENTED_EDGE ( 'NONE', *, *, #5955, .F. ) ;
#10144 = ORIENTED_EDGE ( 'NONE', *, *, #10355, .T. ) ;
#10145 = EDGE_CURVE ( 'NONE', #1872, #11418, #6644, .T. ) ;
#10146 = LINE ( 'NONE', #1955, #2317 ) ;
#10147 = DIRECTION ( 'NONE',  ( 0.000000000000000000, 0.000000000000000000, 1.000000000000000000 ) ) ;
#10148 = CARTESIAN_POINT ( 'NONE',  ( -226.6392846543355688, 19.96883746039994278, 130.8783844631124680 ) ) ;
#10149 = CARTESIAN_POINT ( 'NONE',  ( -239.4316592316125707, -1.761224060149568116, -11.87005020869884220 ) ) ;
#10150 = DIRECTION ( 'NONE',  ( 1.000000000000000000, 0.000000000000000000, 0.000000000000000000 ) ) ;
#10151 = CARTESIAN_POINT ( 'NONE',  ( -244.2512373980594305, 8.280505324206091089, 8.336413190213974644 ) ) ;
#10152 = ORIENTED_EDGE ( 'NONE', *, *, #9658, .F. ) ;
#10153 = CARTESIAN_POINT ( 'NONE',  ( 234.0054343868618503, 20.79694577634646180, 115.4021059068217596 ) ) ;
#10154 = ORIENTED_EDGE ( 'NONE', *, *, #12911, .T. ) ;
#10155 = DIRECTION ( 'NONE',  ( 0.000000000000000000, 0.000000000000000000, -1.000000000000000000 ) ) ;
#10156 = VERTEX_POINT ( 'NONE', #12247 ) ;
#10157 = CONICAL_SURFACE ( 'NONE', #11872, 5.500000000000005329, 0.7853981633974461696 ) ;
#10158 = CARTESIAN_POINT ( 'NONE',  ( 227.3999999999999773, 0.000000000000000000, 0.000000000000000000 ) ) ;
#10159 = CARTESIAN_POINT ( 'NONE',  ( 0.000000000000000000, 30.00000000000000000, 213.5000000000000000 ) ) ;
#10160 = DIRECTION ( 'NONE',  ( -0.000000000000000000, -1.000000000000000000, 0.000000000000000000 ) ) ;
#10161 = DIRECTION ( 'NONE',  ( 1.000000000000000000, 0.000000000000000000, 0.000000000000000000 ) ) ;
#10162 = CARTESIAN_POINT ( 'NONE',  ( -243.9837273761027916, 20.08915143297736705, -91.83222442980269307 ) ) ;
#10163 = PRODUCT_DEFINITION_SHAPE ( 'NONE', 'NONE',  #13132 ) ;
#10164 = DIRECTION ( 'NONE',  ( 0.000000000000000000, 0.000000000000000000, 1.000000000000000000 ) ) ;
#10165 = CARTESIAN_POINT ( 'NONE',  ( -107.6783259591032333, 20.79694577634646535, 237.6585102388684732 ) ) ;
#10166 = EDGE_LOOP ( 'NONE', ( #12079, #6113 ) ) ;
#10167 = CARTESIAN_POINT ( 'NONE',  ( -239.3871161074123961, -1.704640323733336738, -11.62580261113903468 ) ) ;
#10168 = EDGE_CURVE ( 'NONE', #2838, #10530, #2805, .T. ) ;
#10169 = ORIENTED_EDGE ( 'NONE', *, *, #2885, .T. ) ;
#10170 = CARTESIAN_POINT ( 'NONE',  ( -249.3819455666839531, 10.64000139048411597, -4.985720160764467224 ) ) ;
#10171 = CARTESIAN_POINT ( 'NONE',  ( -247.8923716104523010, -9.795774998258135469, -6.931293060606263268 ) ) ;
#10172 = CARTESIAN_POINT ( 'NONE',  ( -249.7928741341071088, -11.67611540586379526, 1.322401171455369173 ) ) ;
#10173 = ORIENTED_EDGE ( 'NONE', *, *, #8174, .T. ) ;
#10174 = AXIS2_PLACEMENT_3D ( 'NONE', #12806, #9729, #4536 ) ;
#10175 = CONICAL_SURFACE ( 'NONE', #4428, 248.7999999999999829, 0.7853981633974348453 ) ;
#10176 = AXIS2_PLACEMENT_3D ( 'NONE', #7080, #4142, #2014 ) ;
#10177 = CARTESIAN_POINT ( 'NONE',  ( -226.3083638773660198, 20.79694577627718388, -130.6873781515817825 ) ) ;
#10178 = CARTESIAN_POINT ( 'NONE',  ( -249.0734550457813725, 9.965425394255507996, -6.685150203396397650 ) ) ;
#10179 = LINE ( 'NONE', #2118, #9754 ) ;
#10180 = CARTESIAN_POINT ( 'NONE',  ( -247.2571636909562756, -9.642662942724268049, -6.714255738455707778 ) ) ;
#10181 = CARTESIAN_POINT ( 'NONE',  ( -245.0843090378622549, 8.789319854609475513, 8.173033110282421632 ) ) ;
#10182 = DIRECTION ( 'NONE',  ( 0.000000000000000000, 1.000000000000000000, 0.000000000000000000 ) ) ;
#10183 = DIRECTION ( 'NONE',  ( 0.4226182617407092668, 0.000000000000000000, -0.9063077870366453848 ) ) ;
#10184 = EDGE_CURVE ( 'NONE', #7991, #2870, #2173, .T. ) ;
#10185 = CARTESIAN_POINT ( 'NONE',  ( 0.000000000000000000, 29.00000000000000000, 195.0000000000000000 ) ) ;
#10186 = EDGE_CURVE ( 'NONE', #11682, #7165, #10263, .T. ) ;
#10187 = CONTEXT_DEPENDENT_SHAPE_REPRESENTATION ( #7492, #3887 ) ;
#10188 = AXIS2_PLACEMENT_3D ( 'NONE', #2845, #6993, #5866 ) ;
#10189 = AXIS2_PLACEMENT_3D ( 'NONE', #290, #7288, #11355 ) ;
#10190 = PLANE ( 'NONE',  #3231 ) ;
#10191 = VERTEX_POINT ( 'NONE', #7311 ) ;
#10192 = ORIENTED_EDGE ( 'NONE', *, *, #4594, .T. ) ;
#10193 = CONICAL_SURFACE ( 'NONE', #11905, 5.100000000000003197, 0.7853981633974503884 ) ;
#10194 = CARTESIAN_POINT ( 'NONE',  ( -258.8746690728235080, 20.08915143284549387, 34.10614053596890471 ) ) ;
#10195 = FACE_OUTER_BOUND ( 'NONE', #12318, .T. ) ;
#10196 = EDGE_CURVE ( 'NONE', #10050, #612, #2180, .T. ) ;
#10197 = PRODUCT_DEFINITION_SHAPE ( 'NONE', 'NONE',  #13091 ) ;
#10198 = CARTESIAN_POINT ( 'NONE',  ( 239.4581646394902918, -1.471889791916103807, -3.175461175216562459 ) ) ;
#10199 = CIRCLE ( 'NONE', #12545, 6.500000000000005329 ) ;
#10200 = CARTESIAN_POINT ( 'NONE',  ( 0.000000000000000000, 11.79660968244690089, 0.000000000000000000 ) ) ;
#10201 = CARTESIAN_POINT ( 'NONE',  ( 259.0935598591524922, 20.79694577673652134, -34.13493237036694694 ) ) ;
#10202 = DIRECTION ( 'NONE',  ( 0.000000000000000000, 0.000000000000000000, -1.000000000000000000 ) ) ;
#10203 = CARTESIAN_POINT ( 'NONE',  ( 0.000000000000000000, 0.000000000000000000, 0.000000000000000000 ) ) ;
#10204 = CARTESIAN_POINT ( 'NONE',  ( -244.4597039952343493, -8.419215818243479532, 8.199143447567463383 ) ) ;
#10205 = ITEM_DEFINED_TRANSFORMATION ( 'NONE', 'NONE', #9118,  #805 ) ;
#10206 = ORIENTED_EDGE ( 'NONE', *, *, #6143, .T. ) ;
#10207 = FACE_BOUND ( 'NONE', #11621, .T. ) ;
#10208 = VECTOR ( 'NONE', #6141, 1000.000000000000000 ) ;
#10209 = CARTESIAN_POINT ( 'NONE',  ( 229.9733680233429993, 8.492964294626340574E-17, 3.499999999999964917 ) ) ;
#10210 = ORIENTED_EDGE ( 'NONE', *, *, #2012, .F. ) ;
#10211 = ORIENTED_EDGE ( 'NONE', *, *, #1678, .F. ) ;
#10212 = VECTOR ( 'NONE', #9906, 1000.000000000000000 ) ;
#10213 = DIRECTION ( 'NONE',  ( -0.000000000000000000, -1.000000000000000000, 0.000000000000000000 ) ) ;
#10214 = DIRECTION ( 'NONE',  ( -0.7071067811865490160, 0.7069694329824840473, -0.01393631330096752920 ) ) ;
#10215 = EDGE_CURVE ( 'NONE', #7040, #2804, #10695, .T. ) ;
#10216 = ADVANCED_FACE ( 'NONE', ( #12111 ), #9621, .F. ) ;
#10217 = CARTESIAN_POINT ( 'NONE',  ( -84.14846197958475216, 19.96883746048893471, -247.8175805193368717 ) ) ;
#10218 = DIRECTION ( 'NONE',  ( 0.000000000000000000, 1.000000000000000000, 0.000000000000000000 ) ) ;
#10219 = CARTESIAN_POINT ( 'NONE',  ( 0.000000000000000000, 0.000000000000000000, 0.000000000000000000 ) ) ;
#10220 = CARTESIAN_POINT ( 'NONE',  ( -241.3883989929918528, 5.445712471069635185, 10.41186067220156097 ) ) ;
#10221 = EDGE_CURVE ( 'NONE', #9610, #4744, #1757, .T. ) ;
#10222 = AXIS2_PLACEMENT_3D ( 'NONE', #8268, #12331, #11330 ) ;
#10223 = ORIENTED_EDGE ( 'NONE', *, *, #2336, .F. ) ;
#10224 = CARTESIAN_POINT ( 'NONE',  ( 59.24444182677519422, 20.79694577634646535, 254.0989678903617346 ) ) ;
#10225 = ORIENTED_EDGE ( 'NONE', *, *, #4481, .F. ) ;
#10226 = AXIS2_PLACEMENT_3D ( 'NONE', #4378, #3434, #7447 ) ;
#10227 = CARTESIAN_POINT ( 'NONE',  ( 0.000000000000000000, 1.848645179567965036, 0.000000000000000000 ) ) ;
#10228 = ORIENTED_EDGE ( 'NONE', *, *, #1396, .F. ) ;
#10229 = CARTESIAN_POINT ( 'NONE',  ( -210.0000000000000000, 30.00000000000000000, 5.100000000000000533 ) ) ;
#10230 = CARTESIAN_POINT ( 'NONE',  ( 0.000000000000000000, 2.772967769359004908, 0.000000000000000000 ) ) ;
#10231 = EDGE_CURVE ( 'NONE', #4889, #3488, #180, .T. ) ;
#10232 = CARTESIAN_POINT ( 'NONE',  ( 238.9743710625075721, 0.08886714786327083726, 3.499996468585938381 ) ) ;
#10233 = CARTESIAN_POINT ( 'NONE',  ( 71.82423009839129691, 28.60000000000000142, 192.2354503650404922 ) ) ;
#10234 = CARTESIAN_POINT ( 'NONE',  ( 0.000000000000000000, 9.830508068689120194, 0.000000000000000000 ) ) ;
#10235 = DIRECTION ( 'NONE',  ( 0.000000000000000000, 1.000000000000000000, 0.000000000000000000 ) ) ;
#10236 = CARTESIAN_POINT ( 'NONE',  ( -258.6823826759385270, 20.79694577634646535, 34.05310945291919467 ) ) ;
#10237 = VERTEX_POINT ( 'NONE', #5307 ) ;
#10238 = DIRECTION ( 'NONE',  ( -0.000000000000000000, -1.000000000000000000, 0.000000000000000000 ) ) ;
#10239 = CIRCLE ( 'NONE', #6842, 0.8000000000000003775 ) ;
#10240 = ADVANCED_FACE ( 'NONE', ( #3787 ), #11010, .T. ) ;
#10241 = ORIENTED_EDGE ( 'NONE', *, *, #6868, .T. ) ;
#10242 = DIRECTION ( 'NONE',  ( 0.000000000000000000, 0.000000000000000000, 1.000000000000000000 ) ) ;
#10243 = CARTESIAN_POINT ( 'NONE',  ( -243.9120028947399987, -8.059256689375558835, -8.893843978839138131 ) ) ;
#10244 = CARTESIAN_POINT ( 'NONE',  ( 8.526617657838109210, 20.08915143297737060, -260.5542428351132571 ) ) ;
#10245 = VERTEX_POINT ( 'NONE', #11381 ) ;
#10246 = TOROIDAL_SURFACE ( 'NONE', #4493, 258.5000000000000000, 2.500000000000035083 ) ;
#10247 = CARTESIAN_POINT ( 'NONE',  ( -17.06760680800445229, 20.79694577634651509, -260.7745447061710138 ) ) ;
#10248 = CARTESIAN_POINT ( 'NONE',  ( -242.3288872988346725, 6.653385920458625868, -9.986615906075055449 ) ) ;
#10249 = CARTESIAN_POINT ( 'NONE',  ( -27.68945685411286561, -29.00000000000000000, 290.6841825403027997 ) ) ;
#10250 = CARTESIAN_POINT ( 'NONE',  ( -242.2664987713461926, -6.571392929281715922, -9.740637196460863123 ) ) ;
#10251 = CARTESIAN_POINT ( 'NONE',  ( -3.647576077974784337, -138.4705547276867321, -41.69198534955605595 ) ) ;
#10252 =( REPRESENTATION_RELATIONSHIP ('NONE','NONE', #12019, #182 ) REPRESENTATION_RELATIONSHIP_WITH_TRANSFORMATION ( #952 )SHAPE_REPRESENTATION_RELATIONSHIP( ) );
#10253 = AXIS2_PLACEMENT_3D ( 'NONE', #6248, #11232, #12173 ) ;
#10254 = CARTESIAN_POINT ( 'NONE',  ( 239.2626306338483460, -1.161280184411060956, 3.302084438360472607 ) ) ;
#10255 = DIRECTION ( 'NONE',  ( 0.8199460427888414227, 0.5538822189107470706, -0.1445786100688019604 ) ) ;
#10256 = DIRECTION ( 'NONE',  ( 0.000000000000000000, 0.000000000000000000, 1.000000000000000000 ) ) ;
#10257 = DIRECTION ( 'NONE',  ( 0.000000000000000000, 0.000000000000000000, 1.000000000000000000 ) ) ;
#10258 = EDGE_LOOP ( 'NONE', ( #8342, #815, #4418, #11164 ) ) ;
#10259 = ORIENTED_EDGE ( 'NONE', *, *, #11245, .F. ) ;
#10260 = CIRCLE ( 'NONE', #7081, 270.0000000000000000 ) ;
#10261 = CARTESIAN_POINT ( 'NONE',  ( -234.1947771728870009, 20.08915143306511553, -115.4648407706533959 ) ) ;
#10262 = CARTESIAN_POINT ( 'NONE',  ( 0.000000000000000000, 24.99999999999995737, 0.000000000000000000 ) ) ;
#10263 = CIRCLE ( 'NONE', #4089, 305.0000000000000000 ) ;
#10264 = ADVANCED_FACE ( 'NONE', ( #10107 ), #10303, .F. ) ;
#10265 = EDGE_CURVE ( 'NONE', #8360, #8155, #3880, .T. ) ;
#10266 = CARTESIAN_POINT ( 'NONE',  ( 239.4538130491200150, -1.465952997496189347, -3.178207852357353591 ) ) ;
#10267 = DIRECTION ( 'NONE',  ( 0.000000000000000000, 1.000000000000000000, 0.000000000000000000 ) ) ;
#10268 = CARTESIAN_POINT ( 'NONE',  ( -249.7118339206215012, -9.997999799959989886, 6.636264009214830395 ) ) ;
#10269 = DIRECTION ( 'NONE',  ( 0.000000000000000000, -1.000000000000000000, 0.000000000000000000 ) ) ;
#10270 = CARTESIAN_POINT ( 'NONE',  ( 0.000000000000000000, 0.000000000000000000, 0.000000000000000000 ) ) ;
#10271 = VECTOR ( 'NONE', #5950, 1000.000000000000000 ) ;
#10272 = CARTESIAN_POINT ( 'NONE',  ( -241.3198063618514482, -5.342363202628128249, 10.46527477498059255 ) ) ;
#10273 = EDGE_LOOP ( 'NONE', ( #12497, #7513, #5213, #7018 ) ) ;
#10274 = MECHANICAL_DESIGN_GEOMETRIC_PRESENTATION_REPRESENTATION (  '', ( #4519 ), #6876 ) ;
#10275 = EDGE_CURVE ( 'NONE', #1858, #9146, #60, .T. ) ;
#10276 = FACE_OUTER_BOUND ( 'NONE', #9888, .T. ) ;
#10277 = ORIENTED_EDGE ( 'NONE', *, *, #870, .T. ) ;
#10278 = ORIENTED_EDGE ( 'NONE', *, *, #12838, .F. ) ;
#10279 = DIRECTION ( 'NONE',  ( 0.000000000000000000, 0.000000000000000000, -1.000000000000000000 ) ) ;
#10280 = DIRECTION ( 'NONE',  ( -0.000000000000000000, -1.000000000000000000, 0.000000000000000000 ) ) ;
#10281 = AXIS2_PLACEMENT_3D ( 'NONE', #10473, #1340, #5409 ) ;
#10282 = AXIS2_PLACEMENT_3D ( 'NONE', #921, #4978, #10915 ) ;
#10283 = CIRCLE ( 'NONE', #11359, 5.500000000000005329 ) ;
#10284 = CARTESIAN_POINT ( 'NONE',  ( -115.7315435907638346, 19.96883745872212046, 234.7354397761344273 ) ) ;
#10285 = CYLINDRICAL_SURFACE ( 'NONE', #12613, 5.500000000000005329 ) ;
#10286 = CONICAL_SURFACE ( 'NONE', #3470, 6.500000000000005329, 0.7853981633974617127 ) ;
#10287 =( NAMED_UNIT ( * ) SI_UNIT ( $, .STERADIAN. ) SOLID_ANGLE_UNIT ( ) );
#10288 = CARTESIAN_POINT ( 'NONE',  ( -241.2214908397801594, 5.194817167650287892, 10.54181336101382271 ) ) ;
#10289 = ORIENTED_EDGE ( 'NONE', *, *, #1008, .F. ) ;
#10290 = CARTESIAN_POINT ( 'NONE',  ( 42.50473797389793873, 20.79694577634646535, 257.4287020129719394 ) ) ;
#10291 = EDGE_CURVE ( 'NONE', #6137, #12985, #8999, .T. ) ;
#10292 = ORIENTED_EDGE ( 'NONE', *, *, #11212, .F. ) ;
#10293 = EDGE_CURVE ( 'NONE', #1100, #4498, #1348, .T. ) ;
#10294 = FACE_OUTER_BOUND ( 'NONE', #5387, .T. ) ;
#10295 = ORIENTED_EDGE ( 'NONE', *, *, #3107, .F. ) ;
#10296 = ORIENTED_EDGE ( 'NONE', *, *, #1321, .T. ) ;
#10297 = DIRECTION ( 'NONE',  ( -0.000000000000000000, -1.000000000000000000, 0.000000000000000000 ) ) ;
#10298 = DIRECTION ( 'NONE',  ( 0.000000000000000000, 0.000000000000000000, 1.000000000000000000 ) ) ;
#10299 = CARTESIAN_POINT ( 'NONE',  ( 239.4470891770647825, 1.456698945264939260, 3.182458632605157600 ) ) ;
#10300 = CARTESIAN_POINT ( 'NONE',  ( 71.82423009839129691, 30.00000000000000000, -197.3354503650404865 ) ) ;
#10301 = AXIS2_PLACEMENT_3D ( 'NONE', #11233, #2101, #6979 ) ;
#10302 = CARTESIAN_POINT ( 'NONE',  ( -237.4577367525703266, 20.08915143297737060, -107.5873595010543511 ) ) ;
#10303 = CYLINDRICAL_SURFACE ( 'NONE', #9835, 5.500000000000005329 ) ;
#10304 = ORIENTED_EDGE ( 'NONE', *, *, #6213, .T. ) ;
#10305 = CONICAL_SURFACE ( 'NONE', #7543, 6.500000000000000888, 0.7853981633974617127 ) ;
#10306 = FACE_OUTER_BOUND ( 'NONE', #11584, .T. ) ;
#10307 = ORIENTED_EDGE ( 'NONE', *, *, #10551, .F. ) ;
#10308 = EDGE_CURVE ( 'NONE', #3933, #2919, #9214, .T. ) ;
#10309 = CARTESIAN_POINT ( 'NONE',  ( -197.8197553893924976, 18.00000000000000000, -64.27553482998719403 ) ) ;
#10310 = CARTESIAN_POINT ( 'NONE',  ( 197.8197553893915028, 30.00000000000000000, -64.27553482998990830 ) ) ;
#10311 = VECTOR ( 'NONE', #3990, 1000.000000000000000 ) ;
#10312 = CARTESIAN_POINT ( 'NONE',  ( -249.7865125415112857, -11.62303781240828648, 1.723091335424036696 ) ) ;
#10313 = ORIENTED_EDGE ( 'NONE', *, *, #4038, .T. ) ;
#10314 = EDGE_CURVE ( 'NONE', #11942, #9651, #1982, .T. ) ;
#10315 = CARTESIAN_POINT ( 'NONE',  ( 130.6873781507030117, 20.79694577677803125, -226.3083638765525052 ) ) ;
#10316 = CARTESIAN_POINT ( 'NONE',  ( -242.3253012572110094, 6.649486011326967372, -9.989214338958454675 ) ) ;
#10317 = CARTESIAN_POINT ( 'NONE',  ( -240.1208361041844910, 2.772967769358974710, 11.41810622433049893 ) ) ;
#10318 = CARTESIAN_POINT ( 'NONE',  ( -243.3200464599152042, -7.587187367930753545, -8.972284967273612466 ) ) ;
#10319 = VECTOR ( 'NONE', #2921, 1000.000000000000000 ) ;
#10320 = CARTESIAN_POINT ( 'NONE',  ( 239.1625895583289605, -0.9513411441973714799, 3.369326940719206576 ) ) ;
#10321 = PRODUCT_DEFINITION_SHAPE ( 'NONE', 'NONE',  #13046 ) ;
#10322 = CARTESIAN_POINT ( 'NONE',  ( 40.42519547187242779, -138.4705547276867321, -10.83189848055806515 ) ) ;
#10323 = CARTESIAN_POINT ( 'NONE',  ( 240.6264023546065971, 3.484414313184070355, -0.3842028184769861743 ) ) ;
#10324 = ITEM_DEFINED_TRANSFORMATION ( 'NONE', 'NONE', #2136,  #805 ) ;
#10325 = DIRECTION ( 'NONE',  ( -0.000000000000000000, 1.000000000000000000, 0.000000000000000000 ) ) ;
#10326 = ORIENTED_EDGE ( 'NONE', *, *, #6811, .F. ) ;
#10327 = VECTOR ( 'NONE', #2513, 1000.000000000000227 ) ;
#10328 = CARTESIAN_POINT ( 'NONE',  ( -260.5542428355875018, 20.08915143288246696, -17.05314194217034895 ) ) ;
#10329 = CARTESIAN_POINT ( 'NONE',  ( 197.8197553893915028, 18.00000000000000000, -64.27553482998990830 ) ) ;
#10330 = AXIS2_PLACEMENT_3D ( 'NONE', #10574, #8585, #3632 ) ;
#10331 = CARTESIAN_POINT ( 'NONE',  ( -248.9866437200756764, 10.23506903978361038, 5.772678316702733348 ) ) ;
#10332 = CARTESIAN_POINT ( 'NONE',  ( 239.1683641398495013, -0.9613626713077001451, -3.365491595546588055 ) ) ;
#10333 = CARTESIAN_POINT ( 'NONE',  ( 197.8197553893915028, 19.00000000000000000, -64.27553482998990830 ) ) ;
#10334 = CARTESIAN_POINT ( 'NONE',  ( -247.9713910029833244, -9.811523844341806466, 6.908981293584625760 ) ) ;
#10335 = CARTESIAN_POINT ( 'NONE',  ( 71.82423009839129691, 18.00000000000000000, -203.8354503650404581 ) ) ;
#10336 = DIRECTION ( 'NONE',  ( 0.8191520442889851372, 0.000000000000000000, 0.5735764363510555963 ) ) ;
#10337 = DIRECTION ( 'NONE',  ( -0.000000000000000000, -1.000000000000000000, 0.000000000000000000 ) ) ;
#10338 = VECTOR ( 'NONE', #5343, 1000.000000000000000 ) ;
#10339 = CONTEXT_DEPENDENT_SHAPE_REPRESENTATION ( #4989, #6134 ) ;
#10340 = ORIENTED_EDGE ( 'NONE', *, *, #2570, .F. ) ;
#10341 = DIRECTION ( 'NONE',  ( 0.000000000000000000, 0.000000000000000000, 1.000000000000000000 ) ) ;
#10342 = EDGE_CURVE ( 'NONE', #12286, #6697, #9108, .T. ) ;
#10343 = CARTESIAN_POINT ( 'NONE',  ( 229.9737195918793873, -0.4604175462015974718, -3.477110600454007994 ) ) ;
#10344 = ORIENTED_EDGE ( 'NONE', *, *, #2754, .F. ) ;
#10345 = ORIENTED_EDGE ( 'NONE', *, *, #6665, .F. ) ;
#10346 = CARTESIAN_POINT ( 'NONE',  ( 240.3826708216974737, -2.772967769359219847, 2.135567781667135012 ) ) ;
#10347 = DIRECTION ( 'NONE',  ( 0.000000000000000000, -1.000000000000000000, 0.000000000000000000 ) ) ;
#10348 = CARTESIAN_POINT ( 'NONE',  ( 259.4723857435292302, 19.96883745945557820, -34.18476129351679305 ) ) ;
#10349 = DIRECTION ( 'NONE',  ( 0.000000000000000000, 1.000000000000000000, 0.000000000000000000 ) ) ;
#10350 = DIRECTION ( 'NONE',  ( 0.7660444431189772363, 0.000000000000000000, 0.6427876096865405842 ) ) ;
#10351 = LINE ( 'NONE', #4543, #7106 ) ;
#10352 = MANIFOLD_SOLID_BREP ( 'NONE', #9226 ) ;
#10353 = EDGE_LOOP ( 'NONE', ( #10411, #5589, #8958, #9353 ) ) ;
#10354 = CARTESIAN_POINT ( 'NONE',  ( 196.1676464792608670, 20.79694577634646535, 172.0303573358521589 ) ) ;
#10355 = EDGE_CURVE ( 'NONE', #9111, #11199, #4099, .T. ) ;
#10356 = EDGE_LOOP ( 'NONE', ( #9252, #8419 ) ) ;
#10357 = CARTESIAN_POINT ( 'NONE',  ( 2.394184492333075617E-14, 19.00000000000000000, 195.0000000000000000 ) ) ;
#10358 = EDGE_LOOP ( 'NONE', ( #12250, #11080, #11095, #924 ) ) ;
#10359 = EDGE_LOOP ( 'NONE', ( #1950, #9563, #6187, #2229 ) ) ;
#10360 =( REPRESENTATION_RELATIONSHIP ('NONE','NONE', #12019, #5191 ) REPRESENTATION_RELATIONSHIP_WITH_TRANSFORMATION ( #8418 )SHAPE_REPRESENTATION_RELATIONSHIP( ) );
#10361 = CARTESIAN_POINT ( 'NONE',  ( 6.735557395310442023E-16, 30.00000000000000000, -213.5000000000000000 ) ) ;
#10362 = DIRECTION ( 'NONE',  ( 0.000000000000000000, 0.000000000000000000, -1.000000000000000000 ) ) ;
#10363 = EDGE_CURVE ( 'NONE', #9436, #10637, #11987, .T. ) ;
#10364 = PRODUCT_DEFINITION_SHAPE ( 'NONE', 'NONE',  #13099 ) ;
#10365 = CARTESIAN_POINT ( 'NONE',  ( 239.2173603368574959, 1.070082898007238326, -3.332413334892890155 ) ) ;
#10366 = CARTESIAN_POINT ( 'NONE',  ( -239.1331760277428771, 1.386671646218362808, -11.66814526318957412 ) ) ;
#10367 = CARTESIAN_POINT ( 'NONE',  ( 0.000000000000000000, -1.848645179579245124, 0.000000000000000000 ) ) ;
#10368 = ITEM_DEFINED_TRANSFORMATION ( 'NONE', 'NONE', #4429,  #805 ) ;
#10369 = ORIENTED_EDGE ( 'NONE', *, *, #12357, .F. ) ;
#10370 = PLANE ( 'NONE',  #4324 ) ;
#10372 = EDGE_LOOP ( 'NONE', ( #6582, #10154 ) ) ;
#10371 = VECTOR ( 'NONE', #2574, 1000.000000000000000 ) ;
#10373 = CARTESIAN_POINT ( 'NONE',  ( -0.000000000000000000, -30.00000000000000000, 0.000000000000000000 ) ) ;
#10374 = CARTESIAN_POINT ( 'NONE',  ( -244.7098307116044111, -8.574293599168578695, -8.395350237759140910 ) ) ;
#10375 = CARTESIAN_POINT ( 'NONE',  ( 151.8458048843644690, 20.08915143297736705, -211.9058003148606417 ) ) ;
#10376 = ORIENTED_EDGE ( 'NONE', *, *, #8183, .F. ) ;
#10377 = CARTESIAN_POINT ( 'NONE',  ( -207.3438552930580272, 20.79694577641581077, -159.0697709843959728 ) ) ;
#10378 = CARTESIAN_POINT ( 'NONE',  ( -241.6809225228018363, 5.875971056241065860, -10.46353150750831063 ) ) ;
#10379 = CARTESIAN_POINT ( 'NONE',  ( -238.9657050040809452, 1.118917709522747828, 11.94772711066928750 ) ) ;
#10380 = EDGE_CURVE ( 'NONE', #6789, #9508, #11962, .T. ) ;
#10381 = CARTESIAN_POINT ( 'NONE',  ( -245.9694114599930401, -9.199502187900977290, -7.310239086664601871 ) ) ;
#10382 = EDGE_CURVE ( 'NONE', #7222, #3384, #7304, .T. ) ;
#10383 =( REPRESENTATION_RELATIONSHIP ('NONE','NONE', #12019, #5191 ) REPRESENTATION_RELATIONSHIP_WITH_TRANSFORMATION ( #3056 )SHAPE_REPRESENTATION_RELATIONSHIP( ) );
#10384 = SURFACE_STYLE_FILL_AREA ( #11398 ) ;
#10385 = SHAPE_DEFINITION_REPRESENTATION ( #8529, #4340 ) ;
#10386 = CARTESIAN_POINT ( 'NONE',  ( 0.000000000000000000, 1.848645179581460019, 0.000000000000000000 ) ) ;
#10387 = ADVANCED_FACE ( 'NONE', ( #511 ), #377, .F. ) ;
#10388 = AXIS2_PLACEMENT_3D ( 'NONE', #11144, #1076, #11207 ) ;
#10389 = CARTESIAN_POINT ( 'NONE',  ( 222.0845275804282153, -1.749660080537334572, 0.03449061573949096376 ) ) ;
#10390 = ORIENTED_EDGE ( 'NONE', *, *, #6249, .F. ) ;
#10391 = CARTESIAN_POINT ( 'NONE',  ( -207.1687172310330141, 20.08915143305816997, -158.9353507251184965 ) ) ;
#10392 = DIRECTION ( 'NONE',  ( 0.000000000000000000, 1.000000000000000000, 0.000000000000000000 ) ) ;
#10393 = CARTESIAN_POINT ( 'NONE',  ( 122.2593324768346008, 19.00000000000000000, 173.7755348299889988 ) ) ;
#10394 = DIRECTION ( 'NONE',  ( 0.000000000000000000, 0.000000000000000000, 1.000000000000000000 ) ) ;
#10395 = EDGE_CURVE ( 'NONE', #368, #11287, #9625, .T. ) ;
#10396 = CARTESIAN_POINT ( 'NONE',  ( 0.000000000000000000, 1.000000000000000000, 0.000000000000000000 ) ) ;
#10397 = AXIS2_PLACEMENT_3D ( 'NONE', #2813, #12757, #5630 ) ;
#10398 = CARTESIAN_POINT ( 'NONE',  ( 229.9000000000000057, 0.000000000000000000, 0.000000000000000000 ) ) ;
#10399 = CONICAL_SURFACE ( 'NONE', #11898, 250.1999999999999602, 0.7853981633974758125 ) ;
#10400 = CARTESIAN_POINT ( 'NONE',  ( 0.000000000000000000, 23.50000000000000000, 0.000000000000000000 ) ) ;
#10401 = CARTESIAN_POINT ( 'NONE',  ( -41.85124196045095601, -138.4705547276867321, -1.461228303123232300E-13 ) ) ;
#10402 = CIRCLE ( 'NONE', #9346, 5.500000000000007994 ) ;
#10403 = DIRECTION ( 'NONE',  ( 0.6368676505102700558, 0.000000000000000000, 0.7709731485165541853 ) ) ;
#10404 = AXIS2_PLACEMENT_3D ( 'NONE', #12421, #3208, #10279 ) ;
#10405 = CONTEXT_DEPENDENT_SHAPE_REPRESENTATION ( #9337, #9003 ) ;
#10406 = ORIENTED_EDGE ( 'NONE', *, *, #3454, .T. ) ;
#10407 = CONICAL_SURFACE ( 'NONE', #2319, 6.500000000000000000, 0.7853981633974518317 ) ;
#10408 = CARTESIAN_POINT ( 'NONE',  ( 240.5378997430557035, -3.246179722999635864, -1.312253685521740598 ) ) ;
#10409 = AXIS2_PLACEMENT_3D ( 'NONE', #8127, #9187, #10051 ) ;
#10410 = CARTESIAN_POINT ( 'NONE',  ( 229.9996576396049193, -3.477719343325218038, 0.4566469936247985473 ) ) ;
#10411 = ORIENTED_EDGE ( 'NONE', *, *, #8934, .F. ) ;
#10412 = ORIENTED_EDGE ( 'NONE', *, *, #13037, .T. ) ;
#10413 = VECTOR ( 'NONE', #1641, 1000.000000000000000 ) ;
#10414 = CARTESIAN_POINT ( 'NONE',  ( -122.2593324768359935, 18.00000000000000000, -174.7755348299880040 ) ) ;
#10415 = FACE_BOUND ( 'NONE', #1745, .T. ) ;
#10416 = PRODUCT_DEFINITION_CONTEXT ( 'detailed design', #3692, 'design' ) ;
#10417 = CARTESIAN_POINT ( 'NONE',  ( 226.6392846532197325, 19.96883746219288724, -130.8783844621844707 ) ) ;
#10418 = CARTESIAN_POINT ( 'NONE',  ( -0.000000000000000000, -11.79660968244695951, 0.000000000000000000 ) ) ;
#10419 = DIRECTION ( 'NONE',  ( -0.5000000000000009992, 0.000000000000000000, 0.8660254037844380415 ) ) ;
#10420 = LINE ( 'NONE', #8434, #5607 ) ;
#10421 = CIRCLE ( 'NONE', #11497, 10.00000000000000888 ) ;
#10422 = MANIFOLD_SOLID_BREP ( 'NONE', #1780 ) ;
#10423 = VERTEX_POINT ( 'NONE', #10440 ) ;
#10424 = DIRECTION ( 'NONE',  ( 1.000000000000000000, 0.000000000000000000, 0.000000000000000000 ) ) ;
#10425 = ORIENTED_EDGE ( 'NONE', *, *, #2626, .F. ) ;
#10426 = DIRECTION ( 'NONE',  ( 0.000000000000000000, -1.000000000000000000, 0.000000000000000000 ) ) ;
#10427 = VERTEX_POINT ( 'NONE', #5442 ) ;
#10428 = EDGE_LOOP ( 'NONE', ( #1902, #6566, #5042, #4762 ) ) ;
#10429 = VECTOR ( 'NONE', #9588, 1000.000000000000000 ) ;
#10430 = DIRECTION ( 'NONE',  ( 0.000000000000000000, 1.000000000000000000, 0.000000000000000000 ) ) ;
#10431 = DIRECTION ( 'NONE',  ( 0.000000000000000000, -1.000000000000000000, 0.000000000000000000 ) ) ;
#10432 = PRODUCT_DEFINITION_SHAPE ( 'NONE', 'NONE',  #13060 ) ;
#10433 = CARTESIAN_POINT ( 'NONE',  ( 3.053044470274350904E-14, -20.00000000000000000, -248.7999999999999829 ) ) ;
#10434 = EDGE_CURVE ( 'NONE', #3580, #2022, #8576, .T. ) ;
#10435 = ADVANCED_FACE ( 'NONE', ( #7571 ), #11644, .F. ) ;
#10436 = CARTESIAN_POINT ( 'NONE',  ( 239.0427084576656114, 0.5779638302498498748, -3.452011086619390934 ) ) ;
#10437 = AXIS2_PLACEMENT_3D ( 'NONE', #3052, #5110, #936 ) ;
#10438 = DIRECTION ( 'NONE',  ( 0.6368676505102708330, 0.000000000000000000, 0.7709731485165535192 ) ) ;
#10439 = CARTESIAN_POINT ( 'NONE',  ( -244.8027971735120047, 8.628165349658024397, 8.339952776931941258 ) ) ;
#10440 = CARTESIAN_POINT ( 'NONE',  ( 158.0678610555357295, -18.00000000000000000, 250.7878554250727632 ) ) ;
#10441 = CIRCLE ( 'NONE', #2352, 250.1999999999999602 ) ;
#10442 = EDGE_LOOP ( 'NONE', ( #9354, #628, #10278, #11317 ) ) ;
#10443 = CARTESIAN_POINT ( 'NONE',  ( 0.000000000000000000, 18.00000000000000000, -208.0000000000000000 ) ) ;
#10444 = ORIENTED_EDGE ( 'NONE', *, *, #3871, .F. ) ;
#10445 = DIRECTION ( 'NONE',  ( -0.6368676505102707219, 0.000000000000000000, -0.7709731485165535192 ) ) ;
#10446 = CYLINDRICAL_SURFACE ( 'NONE', #6180, 5.100000000000000533 ) ;
#10447 = PRODUCT_DEFINITION ( 'UNKNOWN', '', #6833, #2279 ) ;
#10448 = AXIS2_PLACEMENT_3D ( 'NONE', #997, #5050, #8138 ) ;
#10449 = CARTESIAN_POINT ( 'NONE',  ( 260.1353576186482996, 20.08915143297736705, -17.05322212017789951 ) ) ;
#10450 = ORIENTED_EDGE ( 'NONE', *, *, #8588, .T. ) ;
#10451 = CYLINDRICAL_SURFACE ( 'NONE', #1276, 195.0000000000000000 ) ;
#10452 = CARTESIAN_POINT ( 'NONE',  ( -243.5181255321104459, 7.757956330428964264, -9.154932349439130590 ) ) ;
#10453 = CARTESIAN_POINT ( 'NONE',  ( -239.6598046819784145, 1.963348620848123893, 11.83831708201935839 ) ) ;
#10454 = APPLICATION_CONTEXT ( 'automotive_design' ) ;
#10455 = CARTESIAN_POINT ( 'NONE',  ( 0.000000000000000000, 19.00000000000000000, 0.000000000000000000 ) ) ;
#10456 = CARTESIAN_POINT ( 'NONE',  ( -289.8128292627096130, -19.40000000000000213, 10.41748504886635907 ) ) ;
#10457 = CARTESIAN_POINT ( 'NONE',  ( 239.2304539310932512, -1.097329039956110419, 3.323615143768106073 ) ) ;
#10458 = SHAPE_DEFINITION_REPRESENTATION ( #11798, #12521 ) ;
#10459 = CARTESIAN_POINT ( 'NONE',  ( -229.7292463621831757, 4.422629786613017977, -11.15695835592746654 ) ) ;
#10460 = EDGE_CURVE ( 'NONE', #1965, #5629, #6674, .T. ) ;
#10461 = CIRCLE ( 'NONE', #4702, 260.1830065359515061 ) ;
#10462 = ADVANCED_FACE ( 'NONE', ( #8641, #12697 ), #12446, .F. ) ;
#10463 = LINE ( 'NONE', #3583, #5519 ) ;
#10464 = ORIENTED_EDGE ( 'NONE', *, *, #7049, .F. ) ;
#10465 = CARTESIAN_POINT ( 'NONE',  ( -249.7894249019889230, 11.77854918022920039, -2.316202908582821074 ) ) ;
#10466 = CARTESIAN_POINT ( 'NONE',  ( -130.8783844633512956, 19.96883746151126360, 226.6392846543344035 ) ) ;
#10467 = DIRECTION ( 'NONE',  ( 0.5469441386039890496, 0.000000000000000000, -0.8371691043312220470 ) ) ;
#10468 = FACE_OUTER_BOUND ( 'NONE', #10258, .T. ) ;
#10469 = PRODUCT_DEFINITION_SHAPE ( 'NONE', 'NONE',  #13189 ) ;
#10470 = LINE ( 'NONE', #1338, #12771 ) ;
#10471 = MANIFOLD_SOLID_BREP ( 'NONE', #8166 ) ;
#10472 = FACE_OUTER_BOUND ( 'NONE', #4637, .T. ) ;
#10473 = CARTESIAN_POINT ( 'NONE',  ( 0.000000000000000000, -2.926905849962176352E-14, 0.000000000000000000 ) ) ;
#10474 = DIRECTION ( 'NONE',  ( -0.1736481776669340227, 0.000000000000000000, 0.9848077530122074652 ) ) ;
#10475 = DIRECTION ( 'NONE',  ( 0.000000000000000000, 0.000000000000000000, 1.000000000000000000 ) ) ;
#10476 = ITEM_DEFINED_TRANSFORMATION ( 'NONE', 'NONE', #12525,  #805 ) ;
#10477 = ORIENTED_EDGE ( 'NONE', *, *, #4837, .F. ) ;
#10478 = TOROIDAL_SURFACE ( 'NONE', #10253, 241.5000000000000000, 2.500000000000000000 ) ;
#10479 = DIRECTION ( 'NONE',  ( 0.000000000000000000, -1.000000000000000000, 0.000000000000000000 ) ) ;
#10480 = EDGE_CURVE ( 'NONE', #11299, #1949, #7514, .T. ) ;
#10481 = CARTESIAN_POINT ( 'NONE',  ( -229.9210444607178658, -10.37910877259903231, 6.034405755772844770 ) ) ;
#10482 = EDGE_LOOP ( 'NONE', ( #1923, #10785 ) ) ;
#10483 = VERTEX_POINT ( 'NONE', #4893 ) ;
#10484 = DIRECTION ( 'NONE',  ( 0.000000000000000000, 0.9998057603070481525, -0.01970892327970899874 ) ) ;
#10485 = CARTESIAN_POINT ( 'NONE',  ( 0.000000000000000000, 25.00000000000000000, 0.000000000000000000 ) ) ;
#10486 = CIRCLE ( 'NONE', #10690, 6.500000000000005329 ) ;
#10487 = EDGE_CURVE ( 'NONE', #8469, #564, #2683, .T. ) ;
#10488 = ADVANCED_BREP_SHAPE_REPRESENTATION ( '', ( #5935, #805 ), #7613 ) ;
#10489 = CONICAL_SURFACE ( 'NONE', #7512, 6.500000000000005329, 0.7853981633974476129 ) ;
#10490 = CARTESIAN_POINT ( 'NONE',  ( -196.8887528224093444, 20.55460285074426707, 172.6991790975775132 ) ) ;
#10491 = CARTESIAN_POINT ( 'NONE',  ( -228.6269314446401211, -19.00000000000000000, 181.7250016321579835 ) ) ;
#10492 = DIRECTION ( 'NONE',  ( -0.8660254037844398178, 0.000000000000000000, 0.4999999999999980016 ) ) ;
#10493 = AXIS2_PLACEMENT_3D ( 'NONE', #5303, #1436, #9375 ) ;
#10494 = CARTESIAN_POINT ( 'NONE',  ( -210.0000000000000000, 19.40000000000000213, -5.100000000000000533 ) ) ;
#10495 = CARTESIAN_POINT ( 'NONE',  ( 227.3999999999999773, -0.1281080013181084831, -6.498737441995811714 ) ) ;
#10496 = ORIENTED_EDGE ( 'NONE', *, *, #5061, .T. ) ;
#10497 = CARTESIAN_POINT ( 'NONE',  ( 178.3611219674585584, 20.79694577634646890, -190.4297758776777698 ) ) ;
#10498 = VERTEX_POINT ( 'NONE', #3696 ) ;
#10499 = CARTESIAN_POINT ( 'NONE',  ( -0.000000000000000000, -22.00000000000000000, 0.000000000000000000 ) ) ;
#10500 = ORIENTED_EDGE ( 'NONE', *, *, #10836, .T. ) ;
#10501 = VERTEX_POINT ( 'NONE', #6906 ) ;
#10502 = CIRCLE ( 'NONE', #5817, 4.500000000000000000 ) ;
#10503 = CARTESIAN_POINT ( 'NONE',  ( 235.4000000000000057, 2.999417280921144346, -0.05912676983912699968 ) ) ;
#10504 = DIRECTION ( 'NONE',  ( -0.6368676505102706109, 0.000000000000000000, -0.7709731485165535192 ) ) ;
#10505 = DIRECTION ( 'NONE',  ( -1.000000000000000000, 0.000000000000000000, 0.000000000000000000 ) ) ;
#10506 = CARTESIAN_POINT ( 'NONE',  ( 224.4939760857161843, -6.051844909775672576, 0.1192985195352710553 ) ) ;
#10507 = CARTESIAN_POINT ( 'NONE',  ( 159.2169126275676945, -3.061616997868385015E-14, 192.7432871291383663 ) ) ;
#10508 = ORIENTED_EDGE ( 'NONE', *, *, #10537, .T. ) ;
#10509 = AXIS2_PLACEMENT_3D ( 'NONE', #12764, #6712, #5699 ) ;
#10510 = DIRECTION ( 'NONE',  ( 0.000000000000000000, 0.000000000000000000, 1.000000000000000000 ) ) ;
#10511 = ORIENTED_EDGE ( 'NONE', *, *, #1724, .T. ) ;
#10512 =( REPRESENTATION_RELATIONSHIP ('NONE','NONE', #12019, #182 ) REPRESENTATION_RELATIONSHIP_WITH_TRANSFORMATION ( #7509 )SHAPE_REPRESENTATION_RELATIONSHIP( ) );
#10513 = DIRECTION ( 'NONE',  ( 0.000000000000000000, 1.000000000000000000, 0.000000000000000000 ) ) ;
#10514 = DIRECTION ( 'NONE',  ( 0.000000000000000000, 1.000000000000000000, 0.000000000000000000 ) ) ;
#10515 = ADVANCED_FACE ( 'NONE', ( #6966 ), #11134, .F. ) ;
#10516 = CARTESIAN_POINT ( 'NONE',  ( 196.0019244007920349, 20.08915143297736705, -171.8850263962754354 ) ) ;
#10517 = AXIS2_PLACEMENT_3D ( 'NONE', #10396, #9408, #11410 ) ;
#10518 = LINE ( 'NONE', #6459, #1702 ) ;
#10519 = CARTESIAN_POINT ( 'NONE',  ( -243.8618317092203824, 8.020662184074344836, -8.926546575949515727 ) ) ;
#10520 = CARTESIAN_POINT ( 'NONE',  ( -238.9057708211122133, 0.9926994598474889742, 11.95893060915291173 ) ) ;
#10521 = AXIS2_PLACEMENT_3D ( 'NONE', #5528, #1404, #1271 ) ;
#10522 = DIRECTION ( 'NONE',  ( 0.000000000000000000, 1.000000000000000000, 0.000000000000000000 ) ) ;
#10523 = DIRECTION ( 'NONE',  ( -0.000000000000000000, -1.000000000000000000, 0.000000000000000000 ) ) ;
#10524 = CARTESIAN_POINT ( 'NONE',  ( 3.647576077974511222, -138.4705547276867321, 41.69198534955607727 ) ) ;
#10525 = CARTESIAN_POINT ( 'NONE',  ( -229.8466474081030526, 8.575819594941270552, -8.402010734614378862 ) ) ;
#10526 = VECTOR ( 'NONE', #5984, 1000.000000000000114 ) ;
#10527 = AXIS2_PLACEMENT_3D ( 'NONE', #12707, #581, #5708 ) ;
#10528 = ADVANCED_FACE ( 'NONE', ( #6774 ), #3890, .F. ) ;
#10529 = FACE_OUTER_BOUND ( 'NONE', #6505, .T. ) ;
#10530 = VERTEX_POINT ( 'NONE', #5971 ) ;
#10531 = CARTESIAN_POINT ( 'NONE',  ( -196.7513681801157759, 19.96883745974439961, 172.5787240288376836 ) ) ;
#10532 = LINE ( 'NONE', #5265, #1371 ) ;
#10533 = CARTESIAN_POINT ( 'NONE',  ( 290.6841825403032544, -30.00000000000000000, 27.68945685411186730 ) ) ;
#10534 = CARTESIAN_POINT ( 'NONE',  ( -4.572608844893758122E-13, 20.79694577634647601, 260.7745447061711275 ) ) ;
#10535 = AXIS2_PLACEMENT_3D ( 'NONE', #3251, #8337, #10256 ) ;
#10536 = CARTESIAN_POINT ( 'NONE',  ( -221.3800702329290857, 20.08915143297736350, 137.6665579279349174 ) ) ;
#10537 = EDGE_CURVE ( 'NONE', #7619, #4563, #6835, .T. ) ;
#10538 = EDGE_CURVE ( 'NONE', #2601, #4466, #7893, .T. ) ;
#10539 = CYLINDRICAL_SURFACE ( 'NONE', #5167, 5.499999999999998224 ) ;
#10540 = DIRECTION ( 'NONE',  ( -0.3420201433256726542, 0.000000000000000000, 0.9396926207859069846 ) ) ;
#10541 = CARTESIAN_POINT ( 'NONE',  ( -246.5049976566707812, -9.406509141698599308, 7.041467213310991013 ) ) ;
#10542 = DIRECTION ( 'NONE',  ( 0.000000000000000000, 1.000000000000000000, 0.000000000000000000 ) ) ;
#10543 = CIRCLE ( 'NONE', #2859, 304.0000000000000000 ) ;
#10544 = PRODUCT_DEFINITION_SHAPE ( 'NONE', 'NONE',  #9065 ) ;
#10545 = CIRCLE ( 'NONE', #10762, 250.1999999999999602 ) ;
#10546 = DIRECTION ( 'NONE',  ( 0.000000000000000000, 0.000000000000000000, 1.000000000000000000 ) ) ;
#10547 = ORIENTED_EDGE ( 'NONE', *, *, #2168, .T. ) ;
#10548 = ORIENTED_EDGE ( 'NONE', *, *, #911, .F. ) ;
#10549 = CARTESIAN_POINT ( 'NONE',  ( 135.8846079354933352, -19.40000000000000213, -256.1940150085812888 ) ) ;
#10550 = FACE_BOUND ( 'NONE', #9213, .T. ) ;
#10551 = EDGE_CURVE ( 'NONE', #2233, #3500, #2608, .T. ) ;
#10552 = CARTESIAN_POINT ( 'NONE',  ( 84.14846197943569450, 19.96883746176665397, 247.8175805191055190 ) ) ;
#10553 = CIRCLE ( 'NONE', #6727, 4.500000000000000000 ) ;
#10554 = EDGE_CURVE ( 'NONE', #8105, #8290, #11782, .T. ) ;
#10555 = DIRECTION ( 'NONE',  ( 1.200864985790633912E-16, -0.1961161351381850160, 0.9805806756909200006 ) ) ;
#10556 = DIRECTION ( 'NONE',  ( -0.9848077530122074652, 0.000000000000000000, -0.1736481776669340227 ) ) ;
#10557 = DIRECTION ( 'NONE',  ( -0.000000000000000000, -1.000000000000000000, 0.000000000000000000 ) ) ;
#10558 = CARTESIAN_POINT ( 'NONE',  ( -252.0229195836992631, 20.79694577634646535, -67.53249125288884613 ) ) ;
#10559 = VERTEX_POINT ( 'NONE', #5899 ) ;
#10560 = CARTESIAN_POINT ( 'NONE',  ( 6.337788322448691496E-13, 20.79694577634647601, -260.7745447061711275 ) ) ;
#10561 = ADVANCED_FACE ( 'NONE', ( #9897 ), #12426, .F. ) ;
#10562 = ORIENTED_EDGE ( 'NONE', *, *, #12061, .T. ) ;
#10563 = DIRECTION ( 'NONE',  ( 0.6368676505102707219, 0.000000000000000000, 0.7709731485165535192 ) ) ;
#10564 = VERTEX_POINT ( 'NONE', #2623 ) ;
#10565 = ORIENTED_EDGE ( 'NONE', *, *, #1363, .T. ) ;
#10566 = DIRECTION ( 'NONE',  ( -0.000000000000000000, -1.000000000000000000, 0.000000000000000000 ) ) ;
#10567 = CARTESIAN_POINT ( 'NONE',  ( 0.000000000000000000, 19.00000000000000000, 0.000000000000000000 ) ) ;
#10568 = CARTESIAN_POINT ( 'NONE',  ( 0.000000000000000000, 25.00000000000000000, 249.2999999999999829 ) ) ;
#10569 = CARTESIAN_POINT ( 'NONE',  ( -221.6213872890270977, -19.00000000000000000, 190.2057062658400923 ) ) ;
#10570 = DIRECTION ( 'NONE',  ( 0.6368676505102689456, 0.000000000000000000, 0.7709731485165549625 ) ) ;
#10571 = ORIENTED_EDGE ( 'NONE', *, *, #3452, .T. ) ;
#10572 = CARTESIAN_POINT ( 'NONE',  ( -251.0000000000000000, 24.99999999999995737, 0.000000000000000000 ) ) ;
#10573 = ORIENTED_EDGE ( 'NONE', *, *, #7741, .T. ) ;
#10574 = CARTESIAN_POINT ( 'NONE',  ( 0.000000000000000000, -1.000000000000000000, 0.000000000000000000 ) ) ;
#10575 = LINE ( 'NONE', #8391, #7874 ) ;
#10576 = CARTESIAN_POINT ( 'NONE',  ( 135.8846079354933352, -30.00000000000000000, -256.1940150085812888 ) ) ;
#10577 = DIRECTION ( 'NONE',  ( 0.000000000000000000, 1.000000000000000000, 0.000000000000000000 ) ) ;
#10578 = AXIS2_PLACEMENT_3D ( 'NONE', #6817, #8874, #4599 ) ;
#10579 = CARTESIAN_POINT ( 'NONE',  ( -197.8197553893909912, 19.00000000000000000, 69.77553482999131518 ) ) ;
#10580 = CARTESIAN_POINT ( 'NONE',  ( -229.7581126986659399, 5.193038857911240314, 10.54715260651565067 ) ) ;
#10581 = EDGE_CURVE ( 'NONE', #4800, #12659, #5511, .T. ) ;
#10582 =( REPRESENTATION_RELATIONSHIP ('NONE','NONE', #12019, #5191 ) REPRESENTATION_RELATIONSHIP_WITH_TRANSFORMATION ( #4930 )SHAPE_REPRESENTATION_RELATIONSHIP( ) );
#10583 = DIRECTION ( 'NONE',  ( -0.000000000000000000, -1.000000000000000000, 0.000000000000000000 ) ) ;
#10584 = CARTESIAN_POINT ( 'NONE',  ( 0.000000000000000000, 0.000000000000000000, 0.000000000000000000 ) ) ;
#10585 = CARTESIAN_POINT ( 'NONE',  ( -229.9292789904498591, 10.55952007275214299, 5.712813050723659636 ) ) ;
#10586 = ITEM_DEFINED_TRANSFORMATION ( 'NONE', 'NONE', #9161,  #805 ) ;
#10587 = CARTESIAN_POINT ( 'NONE',  ( 0.000000000000000000, 29.00000000000000000, 0.000000000000000000 ) ) ;
#10588 = EDGE_LOOP ( 'NONE', ( #485, #3778, #11392, #12164 ) ) ;
#10589 = CARTESIAN_POINT ( 'NONE',  ( 247.8175805195787689, 19.96883746176681740, 84.14846197955617413 ) ) ;
#10590 = CARTESIAN_POINT ( 'NONE',  ( 0.000000000000000000, -2.926905849962176352E-14, -239.0000000000000000 ) ) ;
#10591 = DIRECTION ( 'NONE',  ( -0.000000000000000000, 0.5169713083949905030, 0.8560027256360646097 ) ) ;
#10592 = DIRECTION ( 'NONE',  ( -0.000000000000000000, -1.000000000000000000, 0.000000000000000000 ) ) ;
#10593 = LINE ( 'NONE', #1468, #1582 ) ;
#10594 = ADVANCED_FACE ( 'NONE', ( #1487 ), #7523, .F. ) ;
#10595 = EDGE_CURVE ( 'NONE', #9991, #11029, #9449, .T. ) ;
#10596 = CARTESIAN_POINT ( 'NONE',  ( 0.000000000000000000, 30.00000000000000000, 196.0000000000000000 ) ) ;
#10597 = CARTESIAN_POINT ( 'NONE',  ( -41.69198534955604885, -138.4705547276867321, 3.647576077974929998 ) ) ;
#10598 = CARTESIAN_POINT ( 'NONE',  ( 0.000000000000000000, 25.00000000000000000, 0.000000000000000000 ) ) ;
#10599 = CONTEXT_DEPENDENT_SHAPE_REPRESENTATION ( #2188, #4952 ) ;
#10600 = AXIS2_PLACEMENT_3D ( 'NONE', #3084, #7163, #6165 ) ;
#10601 = CARTESIAN_POINT ( 'NONE',  ( -242.2998418224420050, -6.621659878705485447, -10.00767884246599415 ) ) ;
#10602 = DIRECTION ( 'NONE',  ( -0.000000000000000000, -1.000000000000000000, 0.000000000000000000 ) ) ;
#10603 = ORIENTED_EDGE ( 'NONE', *, *, #2479, .T. ) ;
#10604 = ORIENTED_EDGE ( 'NONE', *, *, #161, .T. ) ;
#10605 = EDGE_CURVE ( 'NONE', #10156, #7690, #9491, .T. ) ;
#10606 = FACE_OUTER_BOUND ( 'NONE', #5418, .T. ) ;
#10607 = CARTESIAN_POINT ( 'NONE',  ( -197.8197553893909912, 19.00000000000000000, 64.27553482999130097 ) ) ;
#10608 = AXIS2_PLACEMENT_3D ( 'NONE', #2149, #892, #6229 ) ;
#10609 = CONICAL_SURFACE ( 'NONE', #1251, 5.500000000000015099, 0.7853981633974461696 ) ;
#10610 = AXIS2_PLACEMENT_3D ( 'NONE', #2723, #8809, #10940 ) ;
#10611 = CIRCLE ( 'NONE', #8490, 5.500000000000015099 ) ;
#10612 = AXIS2_PLACEMENT_3D ( 'NONE', #12217, #6019, #12603 ) ;
#10613 = CONICAL_SURFACE ( 'NONE', #4865, 5.100000000000017408, 0.7853981633974503884 ) ;
#10614 = CARTESIAN_POINT ( 'NONE',  ( -34.20858920326337227, 20.55460285088512506, -259.6535381484778782 ) ) ;
#10615 = CYLINDRICAL_SURFACE ( 'NONE', #6450, 5.100000000000017408 ) ;
#10616 = DIRECTION ( 'NONE',  ( -0.6427876096865353661, 0.000000000000000000, -0.7660444431189813441 ) ) ;
#10617 = CARTESIAN_POINT ( 'NONE',  ( -240.7431671954870183, 4.340241520815121490, 10.91924886820501683 ) ) ;
#10618 = CARTESIAN_POINT ( 'NONE',  ( -59.24444182677529369, 20.79694577634646890, 254.0989678903616777 ) ) ;
#10619 = ORIENTED_EDGE ( 'NONE', *, *, #12408, .T. ) ;
#10620 = FACE_BOUND ( 'NONE', #7169, .T. ) ;
#10622 = ORIENTED_EDGE ( 'NONE', *, *, #11108, .F. ) ;
#10621 = VECTOR ( 'NONE', #8794, 1000.000000000000000 ) ;
#10623 = CARTESIAN_POINT ( 'NONE',  ( 150.6801963096165764, -30.00000000000000000, 241.8445669022807181 ) ) ;
#10624 = VERTEX_POINT ( 'NONE', #427 ) ;
#10625 = ORIENTED_EDGE ( 'NONE', *, *, #1183, .F. ) ;
#10626 = EDGE_CURVE ( 'NONE', #12676, #789, #10351, .T. ) ;
#10627 = EDGE_CURVE ( 'NONE', #1045, #2184, #1295, .T. ) ;
#10628 = TOROIDAL_SURFACE ( 'NONE', #8714, 241.5000000000000000, 2.500000000000000000 ) ;
#10629 = AXIS2_PLACEMENT_3D ( 'NONE', #9921, #8789, #11993 ) ;
#10630 = CYLINDRICAL_SURFACE ( 'NONE', #720, 305.0000000000000000 ) ;
#10631 = CARTESIAN_POINT ( 'NONE',  ( -0.000000000000000000, -9.830508068730530624, 0.000000000000000000 ) ) ;
#10632 = CARTESIAN_POINT ( 'NONE',  ( 239.7229759539578140, 1.780302303981533552, -3.014465403428259194 ) ) ;
#10633 = CIRCLE ( 'NONE', #8936, 270.0000000000000000 ) ;
#10634 = CARTESIAN_POINT ( 'NONE',  ( -238.9359252207569853, 1.030933083257997707, -11.70468920303632743 ) ) ;
#10635 = DIRECTION ( 'NONE',  ( 1.000000000000000000, 0.000000000000000000, 0.000000000000000000 ) ) ;
#10636 = DIRECTION ( 'NONE',  ( 0.000000000000000000, 0.000000000000000000, 1.000000000000000000 ) ) ;
#10637 = VERTEX_POINT ( 'NONE', #3278 ) ;
#10638 = CARTESIAN_POINT ( 'NONE',  ( -238.9184900493855821, -0.9919588255939099097, 11.70805706110242106 ) ) ;
#10639 = ORIENTED_EDGE ( 'NONE', *, *, #10551, .T. ) ;
#10640 = CARTESIAN_POINT ( 'NONE',  ( -240.7240246250781013, 4.307698618653014400, -10.93373802373241688 ) ) ;
#10641 = LINE ( 'NONE', #12704, #4069 ) ;
#10642 = AXIS2_PLACEMENT_3D ( 'NONE', #4684, #10694, #7761 ) ;
#10643 = ADVANCED_FACE ( 'NONE', ( #12553 ), #4751, .F. ) ;
#10644 = CARTESIAN_POINT ( 'NONE',  ( 227.3999999999999773, -0.1281080013181084831, -6.498737441995811714 ) ) ;
#10645 = CARTESIAN_POINT ( 'NONE',  ( 153.9282213272189495, -18.00000000000000000, 245.7765299597151341 ) ) ;
#10646 = CARTESIAN_POINT ( 'NONE',  ( -239.2640814428857539, 1.577485845743592741, 11.89585958266493471 ) ) ;
#10647 = CARTESIAN_POINT ( 'NONE',  ( -229.8886654188676744, 9.323152609548129632, 7.161763144159140282 ) ) ;
#10648 = CARTESIAN_POINT ( 'NONE',  ( 182.4625818711949137, -19.00000000000000000, 220.8838070499906223 ) ) ;
#10649 = CARTESIAN_POINT ( 'NONE',  ( 140.0242476638101152, -30.00000000000000000, -251.1826895432237166 ) ) ;
#10650 = SHAPE_DEFINITION_REPRESENTATION ( #11399, #12019 ) ;
#10651 = LINE ( 'NONE', #3644, #3074 ) ;
#10652 = CONTEXT_DEPENDENT_SHAPE_REPRESENTATION ( #6561, #12486 ) ;
#10653 = AXIS2_PLACEMENT_3D ( 'NONE', #10524, #7392, #11460 ) ;
#10654 = EDGE_LOOP ( 'NONE', ( #9817, #727, #4998, #5262 ) ) ;
#10655 = CARTESIAN_POINT ( 'NONE',  ( 3.080812409053027094E-14, 24.75600756274008063, 251.5674242726970817 ) ) ;
#10656 = EDGE_LOOP ( 'NONE', ( #11087, #11100, #827, #8834 ) ) ;
#10657 = CARTESIAN_POINT ( 'NONE',  ( -207.6469600138974272, 19.96883745988519365, -159.3024069661565534 ) ) ;
#10658 = DIRECTION ( 'NONE',  ( 1.000000000000000000, 0.000000000000000000, 0.000000000000000000 ) ) ;
#10659 = PLANE ( 'NONE',  #932 ) ;
#10660 = DIRECTION ( 'NONE',  ( -0.000000000000000000, -1.000000000000000000, 0.000000000000000000 ) ) ;
#10661 = AXIS2_PLACEMENT_3D ( 'NONE', #10584, #2452, #1394 ) ;
#10662 = FACE_BOUND ( 'NONE', #6027, .T. ) ;
#10663 = DIRECTION ( 'NONE',  ( 0.000000000000000000, 0.9998057603070481525, -0.01970892327970899874 ) ) ;
#10664 = DIRECTION ( 'NONE',  ( 0.8191520442889910214, 0.000000000000000000, 0.5735764363510471586 ) ) ;
#10665 = CARTESIAN_POINT ( 'NONE',  ( -229.9163773335792484, -9.982439288020907853, -6.209883811240605844 ) ) ;
#10666 = CARTESIAN_POINT ( 'NONE',  ( 0.000000000000000000, 29.00000000000000000, 0.000000000000000000 ) ) ;
#10667 = CIRCLE ( 'NONE', #4924, 6.500000000000005329 ) ;
#10668 = AXIS2_PLACEMENT_3D ( 'NONE', #10807, #5746, #9802 ) ;
#10669 = CARTESIAN_POINT ( 'NONE',  ( -289.8128292627096130, -19.40000000000000213, 10.41748504886635907 ) ) ;
#10670 = VERTEX_POINT ( 'NONE', #7363 ) ;
#10671 = EDGE_CURVE ( 'NONE', #5366, #4597, #6683, .T. ) ;
#10672 = ORIENTED_EDGE ( 'NONE', *, *, #1874, .F. ) ;
#10673 = EDGE_CURVE ( 'NONE', #7200, #12258, #10283, .T. ) ;
#10674 = DIRECTION ( 'NONE',  ( 0.6368676505102700558, 0.000000000000000000, 0.7709731485165541853 ) ) ;
#10675 = FACE_BOUND ( 'NONE', #9813, .T. ) ;
#10676 = CARTESIAN_POINT ( 'NONE',  ( -1.010328782420808020E-12, 20.79694577634649022, 260.7745447061710138 ) ) ;
#10677 = DIRECTION ( 'NONE',  ( 0.000000000000000000, 0.000000000000000000, 1.000000000000000000 ) ) ;
#10678 =( REPRESENTATION_RELATIONSHIP ('NONE','NONE', #12019, #5191 ) REPRESENTATION_RELATIONSHIP_WITH_TRANSFORMATION ( #9773 )SHAPE_REPRESENTATION_RELATIONSHIP( ) );
#10679 = PRODUCT_DEFINITION_SHAPE ( 'NONE', 'NONE',  #13188 ) ;
#10680 = DIRECTION ( 'NONE',  ( -0.9063077870366481603, 0.000000000000000000, -0.4226182617407033271 ) ) ;
#10681 = DIRECTION ( 'NONE',  ( 0.000000000000000000, 0.000000000000000000, 1.000000000000000000 ) ) ;
#10682 = AXIS2_PLACEMENT_3D ( 'NONE', #11107, #5237, #9307 ) ;
#10683 = FACE_OUTER_BOUND ( 'NONE', #6827, .T. ) ;
#10684 = ORIENTED_EDGE ( 'NONE', *, *, #5760, .F. ) ;
#10685 = DIRECTION ( 'NONE',  ( -0.000000000000000000, 1.000000000000000000, 0.000000000000000000 ) ) ;
#10686 = EDGE_LOOP ( 'NONE', ( #807, #4709 ) ) ;
#10687 = CARTESIAN_POINT ( 'NONE',  ( 190.1049936773181628, -30.00000000000000000, 230.1354848321892632 ) ) ;
#10688 = VERTEX_POINT ( 'NONE', #3481 ) ;
#10689 = EDGE_LOOP ( 'NONE', ( #5112, #6320, #3416, #3669 ) ) ;
#10690 = AXIS2_PLACEMENT_3D ( 'NONE', #2918, #12802, #7004 ) ;
#10691 = VERTEX_POINT ( 'NONE', #12685 ) ;
#10692 = CONICAL_SURFACE ( 'NONE', #4509, 6.500000000000005329, 0.7853981633974617127 ) ;
#10693 = FACE_OUTER_BOUND ( 'NONE', #8889, .T. ) ;
#10694 = DIRECTION ( 'NONE',  ( 0.000000000000000000, 1.000000000000000000, 0.000000000000000000 ) ) ;
#10695 = CIRCLE ( 'NONE', #7295, 239.0000000000000000 ) ;
#10696 =( REPRESENTATION_RELATIONSHIP ('NONE','NONE', #12019, #5191 ) REPRESENTATION_RELATIONSHIP_WITH_TRANSFORMATION ( #1539 )SHAPE_REPRESENTATION_RELATIONSHIP( ) );
#10697 = CARTESIAN_POINT ( 'NONE',  ( -158.9353507255915190, 20.08915143292644245, -207.1687172315094756 ) ) ;
#10698 = CYLINDRICAL_SURFACE ( 'NONE', #528, 249.7999999999999829 ) ;
#10699 = DIRECTION ( 'NONE',  ( 0.6368676505102707219, 0.000000000000000000, 0.7709731485165535192 ) ) ;
#10700 = EDGE_CURVE ( 'NONE', #10427, #2005, #7949, .T. ) ;
#10701 = EDGE_CURVE ( 'NONE', #4344, #8755, #9642, .T. ) ;
#10702 = CONTEXT_DEPENDENT_SHAPE_REPRESENTATION ( #2742, #5198 ) ;
#10703 = ORIENTED_EDGE ( 'NONE', *, *, #6665, .T. ) ;
#10704 = DIRECTION ( 'NONE',  ( -0.000000000000000000, -1.000000000000000000, 0.000000000000000000 ) ) ;
#10705 = AXIS2_PLACEMENT_3D ( 'NONE', #4202, #7474, #11547 ) ;
#10706 = VERTEX_POINT ( 'NONE', #6363 ) ;
#10707 = AXIS2_PLACEMENT_3D ( 'NONE', #9244, #8252, #2241 ) ;
#10708 = CARTESIAN_POINT ( 'NONE',  ( -244.2081860509996716, 8.251870590816803741, -8.364754207297883326 ) ) ;
#10709 = FACE_OUTER_BOUND ( 'NONE', #1843, .T. ) ;
#10710 = DIRECTION ( 'NONE',  ( 0.6368676505102696117, 0.000000000000000000, 0.7709731485165545184 ) ) ;
#10711 = DIRECTION ( 'NONE',  ( 0.000000000000000000, 0.9998057603070481525, -0.01970892327970899527 ) ) ;
#10712 = DIRECTION ( 'NONE',  ( 0.6368676505102716101, 0.000000000000000000, 0.7709731485165527420 ) ) ;
#10713 = AXIS2_PLACEMENT_3D ( 'NONE', #1568, #7817, #11892 ) ;
#10714 = DIRECTION ( 'NONE',  ( 1.000000000000000000, 0.000000000000000000, 0.000000000000000000 ) ) ;
#10715 = VECTOR ( 'NONE', #3167, 1000.000000000000000 ) ;
#10716 = AXIS2_PLACEMENT_3D ( 'NONE', #8879, #12942, #3811 ) ;
#10717 = CARTESIAN_POINT ( 'NONE',  ( -290.6841825403030839, -30.00000000000000000, -27.68945685411394919 ) ) ;
#10718 = EDGE_CURVE ( 'NONE', #5331, #5784, #10420, .T. ) ;
#10719 = DIRECTION ( 'NONE',  ( 0.6368676505102707219, 0.000000000000000000, 0.7709731485165536302 ) ) ;
#10720 = CONTEXT_DEPENDENT_SHAPE_REPRESENTATION ( #9405, #11507 ) ;
#10721 = CARTESIAN_POINT ( 'NONE',  ( -229.9710684506134157, 11.43264861468415816, 3.665441760567183405 ) ) ;
#10722 = EDGE_LOOP ( 'NONE', ( #4917, #6517, #4243, #5279 ) ) ;
#10723 = VECTOR ( 'NONE', #10094, 1000.000000000000114 ) ;
#10724 = EDGE_CURVE ( 'NONE', #90, #1703, #2198, .T. ) ;
#10725 = EDGE_LOOP ( 'NONE', ( #1981, #4692, #712, #2216 ) ) ;
#10726 = CARTESIAN_POINT ( 'NONE',  ( -248.0831933713610056, 9.830508068705238856, 6.436117704883899115 ) ) ;
#10727 = EDGE_LOOP ( 'NONE', ( #13022, #10277 ) ) ;
#10728 = CARTESIAN_POINT ( 'NONE',  ( 34.18476129304277578, 19.96883745937039834, 259.4723857425807978 ) ) ;
#10729 = CARTESIAN_POINT ( 'NONE',  ( 122.2593324768346008, 29.00000000000000000, 162.7755348299889988 ) ) ;
#10730 = DIRECTION ( 'NONE',  ( 1.000000000000000000, 0.000000000000000000, 0.000000000000000000 ) ) ;
#10731 = CARTESIAN_POINT ( 'NONE',  ( -240.9204428197673451, 4.702057767962908308, 11.04114865026916270 ) ) ;
#10732 = CIRCLE ( 'NONE', #8608, 2.250000000000000000 ) ;
#10733 = CARTESIAN_POINT ( 'NONE',  ( -233.0000000000000000, 0.000000000000000000, 0.000000000000000000 ) ) ;
#10734 = DIRECTION ( 'NONE',  ( 5.813980035187680120E-15, 0.5538822189107472926, -0.8325950321581960800 ) ) ;
#10735 = CARTESIAN_POINT ( 'NONE',  ( 229.9784876240037477, 1.548910481047297560, -3.146875811102413767 ) ) ;
#10736 = ITEM_DEFINED_TRANSFORMATION ( 'NONE', 'NONE', #10017,  #805 ) ;
#10737 = CARTESIAN_POINT ( 'NONE',  ( -248.9847817899753295, 10.23580904479008602, -5.770128482949556492 ) ) ;
#10738 = CARTESIAN_POINT ( 'NONE',  ( -240.4848270099879528, -3.809198625046382070, -11.37937944660441048 ) ) ;
#10739 = CARTESIAN_POINT ( 'NONE',  ( -197.8197553893909912, 18.00000000000000000, 57.77553482999131518 ) ) ;
#10740 = ORIENTED_EDGE ( 'NONE', *, *, #11991, .T. ) ;
#10741 = ORIENTED_EDGE ( 'NONE', *, *, #9218, .T. ) ;
#10742 = AXIS2_PLACEMENT_3D ( 'NONE', #12653, #5654, #9849 ) ;
#10743 = FACE_OUTER_BOUND ( 'NONE', #6911, .T. ) ;
#10744 = FACE_BOUND ( 'NONE', #10958, .T. ) ;
#10745 = CARTESIAN_POINT ( 'NONE',  ( -67.61424743051179576, 20.79694577629433283, 252.4341100433384781 ) ) ;
#10746 = CARTESIAN_POINT ( 'NONE',  ( -239.8125244184153644, -2.098251440017480540, -11.56389750598835953 ) ) ;
#10747 = DIRECTION ( 'NONE',  ( -3.491481338843133355E-15, 0.000000000000000000, 1.000000000000000000 ) ) ;
#10748 = DIRECTION ( 'NONE',  ( 0.000000000000000000, 0.000000000000000000, 1.000000000000000000 ) ) ;
#10749 = CARTESIAN_POINT ( 'NONE',  ( 197.8197553893915028, 30.00000000000000000, -57.77553482998990830 ) ) ;
#10750 = EDGE_CURVE ( 'NONE', #6828, #3737, #6432, .T. ) ;
#10751 = AXIS2_PLACEMENT_3D ( 'NONE', #5001, #9597, #7941 ) ;
#10752 = VERTEX_POINT ( 'NONE', #7617 ) ;
#10753 = CARTESIAN_POINT ( 'NONE',  ( 229.9000000000000057, -3.924178331435803635, 2.975033516296866853 ) ) ;
#10754 = ORIENTED_EDGE ( 'NONE', *, *, #8682, .F. ) ;
#10755 = ORIENTED_EDGE ( 'NONE', *, *, #12101, .T. ) ;
#10756 = CARTESIAN_POINT ( 'NONE',  ( 190.2689011420770271, 20.08915143297736705, 178.2104428091928696 ) ) ;
#10757 = VERTEX_POINT ( 'NONE', #8495 ) ;
#10758 = AXIS2_PLACEMENT_3D ( 'NONE', #689, #5752, #6626 ) ;
#10759 = FACE_OUTER_BOUND ( 'NONE', #8485, .T. ) ;
#10760 = CARTESIAN_POINT ( 'NONE',  ( 194.2446334056325554, 0.000000000000000000, 235.1468102975488250 ) ) ;
#10761 =( REPRESENTATION_RELATIONSHIP ('NONE','NONE', #12019, #182 ) REPRESENTATION_RELATIONSHIP_WITH_TRANSFORMATION ( #5241 )SHAPE_REPRESENTATION_RELATIONSHIP( ) );
#10762 = AXIS2_PLACEMENT_3D ( 'NONE', #11432, #2288, #4096 ) ;
#10763 = DIRECTION ( 'NONE',  ( 0.000000000000000000, 1.000000000000000000, 0.000000000000000000 ) ) ;
#10764 = DIRECTION ( 'NONE',  ( -0.6368676505102707219, 0.000000000000000000, -0.7709731485165535192 ) ) ;
#10765 = DIRECTION ( 'NONE',  ( 0.000000000000000000, 0.000000000000000000, 1.000000000000000000 ) ) ;
#10766 = DIRECTION ( 'NONE',  ( -1.000000000000000000, 0.000000000000000000, 0.000000000000000000 ) ) ;
#10767 = ITEM_DEFINED_TRANSFORMATION ( 'NONE', 'NONE', #2928,  #805 ) ;
#10768 = VERTEX_POINT ( 'NONE', #11694 ) ;
#10769 = FACE_OUTER_BOUND ( 'NONE', #2890, .T. ) ;
#10770 = ORIENTED_EDGE ( 'NONE', *, *, #5754, .T. ) ;
#10771 = CARTESIAN_POINT ( 'NONE',  ( 122.2593324768346008, 19.00000000000000000, 168.2755348299889988 ) ) ;
#10772 = ORIENTED_EDGE ( 'NONE', *, *, #5816, .F. ) ;
#10773 = ADVANCED_FACE ( 'NONE', ( #11563 ), #10892, .F. ) ;
#10774 = CARTESIAN_POINT ( 'NONE',  ( 240.3826708216964789, -2.772967769359314882, -2.135567781667015108 ) ) ;
#10775 = FACE_OUTER_BOUND ( 'NONE', #11519, .T. ) ;
#10776 = DIRECTION ( 'NONE',  ( 0.6368676505102716101, 0.000000000000000000, 0.7709731485165527420 ) ) ;
#10777 = FACE_OUTER_BOUND ( 'NONE', #8231, .T. ) ;
#10778 = CARTESIAN_POINT ( 'NONE',  ( -240.2579444296266615, -3.284593558526797352, 11.55663755358773415 ) ) ;
#10779 = DIRECTION ( 'NONE',  ( 0.000000000000000000, -0.9998057603070480415, 0.01970892327970912364 ) ) ;
#10780 = ORIENTED_EDGE ( 'NONE', *, *, #946, .F. ) ;
#10781 = CARTESIAN_POINT ( 'NONE',  ( -229.7551259172103357, 5.607610899293940854, 10.61085097052528425 ) ) ;
#10782 = EDGE_LOOP ( 'NONE', ( #9922, #8919, #10304, #9760 ) ) ;
#10783 = ORIENTED_EDGE ( 'NONE', *, *, #3452, .F. ) ;
#10784 = CARTESIAN_POINT ( 'NONE',  ( -249.6387411365544438, -11.08439570779736805, -3.900217601532822265 ) ) ;
#10785 = ORIENTED_EDGE ( 'NONE', *, *, #9567, .F. ) ;
#10786 = ADVANCED_FACE ( 'NONE', ( #560 ), #759, .F. ) ;
#10787 = CARTESIAN_POINT ( 'NONE',  ( -84.20717312421410838, 20.55460285060721048, -247.9906035374705766 ) ) ;
#10788 = ADVANCED_FACE ( 'NONE', ( #8818 ), #8803, .F. ) ;
#10789 = DIRECTION ( 'NONE',  ( 0.000000000000000000, 0.000000000000000000, -1.000000000000000000 ) ) ;
#10790 = FACE_OUTER_BOUND ( 'NONE', #4132, .T. ) ;
#10791 = DIRECTION ( 'NONE',  ( 0.000000000000000000, 0.000000000000000000, 1.000000000000000000 ) ) ;
#10792 = CARTESIAN_POINT ( 'NONE',  ( 0.000000000000000000, -11.79660968244690089, 0.000000000000000000 ) ) ;
#10793 = EDGE_CURVE ( 'NONE', #1691, #5366, #12811, .T. ) ;
#10794 = LINE ( 'NONE', #742, #11327 ) ;
#10795 = DIRECTION ( 'NONE',  ( 0.4775568914688882449, 0.5538822189107472926, -0.6820219226572412641 ) ) ;
#10796 = CARTESIAN_POINT ( 'NONE',  ( -229.9251749084369010, -10.18240290800271808, -5.876142929606890775 ) ) ;
#10797 = CONTEXT_DEPENDENT_SHAPE_REPRESENTATION ( #11952, #7710 ) ;
#10798 = PRODUCT_DEFINITION_SHAPE ( 'NONE', 'NONE',  #13144 ) ;
#10799 = CARTESIAN_POINT ( 'NONE',  ( -248.8285144558675768, 10.12619208588392716, -5.960099103720946978 ) ) ;
#10800 = DIRECTION ( 'NONE',  ( -0.000000000000000000, -1.000000000000000000, 0.000000000000000000 ) ) ;
#10801 = AXIS2_PLACEMENT_3D ( 'NONE', #599, #6937, #9716 ) ;
#10802 = CARTESIAN_POINT ( 'NONE',  ( 122.2593324768346008, 30.00000000000000000, 173.7755348299889988 ) ) ;
#10803 = ORIENTED_EDGE ( 'NONE', *, *, #2626, .T. ) ;
#10804 = ORIENTED_EDGE ( 'NONE', *, *, #9486, .T. ) ;
#10805 = DIRECTION ( 'NONE',  ( 0.000000000000000000, -1.000000000000000000, 0.000000000000000000 ) ) ;
#10806 = EDGE_CURVE ( 'NONE', #8298, #4613, #4672, .T. ) ;
#10807 = CARTESIAN_POINT ( 'NONE',  ( 71.82423009839129691, 19.40000000000000213, 197.3354503650404865 ) ) ;
#10808 = CARTESIAN_POINT ( 'NONE',  ( -226.3083638773660198, 20.79694577627718388, -130.6873781515817825 ) ) ;
#10809 = CARTESIAN_POINT ( 'NONE',  ( 227.3999999999999773, 0.000000000000000000, 0.000000000000000000 ) ) ;
#10810 = DIRECTION ( 'NONE',  ( -0.9961946980917451011, 0.000000000000000000, -0.08715574274766503537 ) ) ;
#10811 = DIRECTION ( 'NONE',  ( 0.000000000000000000, 0.000000000000000000, 1.000000000000000000 ) ) ;
#10812 = DIRECTION ( 'NONE',  ( 0.000000000000000000, 0.9998057603070481525, -0.01970892327970900221 ) ) ;
#10813 = EDGE_LOOP ( 'NONE', ( #9368, #6666, #3633, #7969 ) ) ;
#10814 = CARTESIAN_POINT ( 'NONE',  ( -238.7981149109900514, -0.6946964185326648389, 11.97987716372956690 ) ) ;
#10815 = ORIENTED_EDGE ( 'NONE', *, *, #10538, .T. ) ;
#10816 = ORIENTED_EDGE ( 'NONE', *, *, #3248, .T. ) ;
#10817 = AXIS2_PLACEMENT_3D ( 'NONE', #10549, #6753, #10674 ) ;
#10818 = AXIS2_PLACEMENT_3D ( 'NONE', #4270, #12413, #3265 ) ;
#10819 = CARTESIAN_POINT ( 'NONE',  ( 91.83222442980259359, 20.08915143297736705, 243.9837273761028769 ) ) ;
#10820 = ORIENTED_EDGE ( 'NONE', *, *, #12302, .T. ) ;
#10821 = LINE ( 'NONE', #10891, #7730 ) ;
#10822 = CARTESIAN_POINT ( 'NONE',  ( -122.2593324768359935, 30.00000000000000000, -168.2755348299880040 ) ) ;
#10823 = CARTESIAN_POINT ( 'NONE',  ( -247.2466869553009872, 20.08915143298854389, 83.95474316008009907 ) ) ;
#10824 = DIRECTION ( 'NONE',  ( 1.000000000000000000, 0.000000000000000000, 0.000000000000000000 ) ) ;
#10825 = DIRECTION ( 'NONE',  ( 0.000000000000000000, 0.000000000000000000, 1.000000000000000000 ) ) ;
#10826 = PRODUCT_DEFINITION_SHAPE ( 'NONE', 'NONE',  #13077 ) ;
#10827 = VECTOR ( 'NONE', #5346, 1000.000000000000000 ) ;
#10828 = ORIENTED_EDGE ( 'NONE', *, *, #9412, .F. ) ;
#10829 = CIRCLE ( 'NONE', #4226, 249.2999999999999829 ) ;
#10830 = LINE ( 'NONE', #7573, #11791 ) ;
#10831 = ORIENTED_EDGE ( 'NONE', *, *, #9987, .F. ) ;
#10832 = CARTESIAN_POINT ( 'NONE',  ( -241.8128863246191997, 6.047237977407489140, -10.08137159590333276 ) ) ;
#10833 = ORIENTED_EDGE ( 'NONE', *, *, #4365, .T. ) ;
#10834 = VECTOR ( 'NONE', #9519, 1000.000000000000000 ) ;
#10835 =( REPRESENTATION_RELATIONSHIP ('NONE','NONE', #12019, #5191 ) REPRESENTATION_RELATIONSHIP_WITH_TRANSFORMATION ( #3662 )SHAPE_REPRESENTATION_RELATIONSHIP( ) );
#10836 = EDGE_CURVE ( 'NONE', #9692, #7101, #295, .T. ) ;
#10837 = ADVANCED_FACE ( 'NONE', ( #3611 ), #3467, .F. ) ;
#10838 = CIRCLE ( 'NONE', #6804, 246.0000000000000000 ) ;
#10839 = DIRECTION ( 'NONE',  ( 0.6368676505102716101, 0.000000000000000000, 0.7709731485165527420 ) ) ;
#10840 = DIRECTION ( 'NONE',  ( 8.659560562354926695E-17, 0.7071067811865480168, -0.7071067811865470176 ) ) ;
#10841 = CARTESIAN_POINT ( 'NONE',  ( -249.7894249019897188, -11.77854918023606601, 2.316202908502521307 ) ) ;
#10842 = CARTESIAN_POINT ( 'NONE',  ( -229.9999671744778880, 11.74935745764778261, 0.7847617075409144549 ) ) ;
#10843 = CIRCLE ( 'NONE', #12336, 6.500000000000005329 ) ;
#10844 = CARTESIAN_POINT ( 'NONE',  ( -245.3145835540676103, -8.904103460292617456, 8.045132556050477390 ) ) ;
#10845 = CARTESIAN_POINT ( 'NONE',  ( -238.7981149122642250, 0.6946964228884829895, -11.97987716347747522 ) ) ;
#10846 = ORIENTED_EDGE ( 'NONE', *, *, #2602, .T. ) ;
#10847 = CARTESIAN_POINT ( 'NONE',  ( -229.7140139254735800, 3.557752282343352945, 11.46654900609709848 ) ) ;
#10848 = VECTOR ( 'NONE', #507, 1000.000000000000000 ) ;
#10849 = ORIENTED_EDGE ( 'NONE', *, *, #763, .T. ) ;
#10850 = AXIS2_PLACEMENT_3D ( 'NONE', #10644, #11454, #2571 ) ;
#10851 = EDGE_LOOP ( 'NONE', ( #7497, #9708, #1719, #9533 ) ) ;
#10852 = CARTESIAN_POINT ( 'NONE',  ( -249.1881502584881787, -10.41621036620467677, -5.437499737166764824 ) ) ;
#10853 = VERTEX_POINT ( 'NONE', #9676 ) ;
#10854 = CARTESIAN_POINT ( 'NONE',  ( 252.9796497720277841, 20.55460285096646089, 67.76049180220992696 ) ) ;
#10855 = DIRECTION ( 'NONE',  ( 0.000000000000000000, -1.000000000000000000, 0.000000000000000000 ) ) ;
#10856 = DIRECTION ( 'NONE',  ( 0.000000000000000000, 1.000000000000000000, 0.000000000000000000 ) ) ;
#10857 = DIRECTION ( 'NONE',  ( 0.000000000000000000, 0.000000000000000000, -1.000000000000000000 ) ) ;
#10858 = CARTESIAN_POINT ( 'NONE',  ( -241.4352517276585104, 5.538320169061370812, 10.64816312846143553 ) ) ;
#10859 = AXIS2_PLACEMENT_3D ( 'NONE', #4722, #3, #3184 ) ;
#10860 = DIRECTION ( 'NONE',  ( 0.000000000000000000, 0.000000000000000000, 1.000000000000000000 ) ) ;
#10861 = CARTESIAN_POINT ( 'NONE',  ( -17.68709912901499237, -138.4705547276867321, -37.93010648591179290 ) ) ;
#10862 = ADVANCED_FACE ( 'NONE', ( #4739 ), #7734, .F. ) ;
#10863 = CARTESIAN_POINT ( 'NONE',  ( 122.2593324768334071, 19.00000000000000000, -162.7755348299894820 ) ) ;
#10864 = B_SPLINE_CURVE_WITH_KNOTS ( 'NONE', 3,
 ( #1472, #7665, #8736, #5535, #12796, #1538, #8612, #3660, #12669, #7731, #5604, #12866, #7602, #6745, #11677, #10665, #10796, #1665, #672, #4723, #8801, #3730, #7796, #7138, #6999, #5051, #3930, #10001, #10997, #1063, #12007, #9002, #8209, #869, #8939, #10065, #6132, #9128, #937, #1809, #73, #4929, #4128, #12132, #3115, #5120, #11194, #2914, #2000 ),
 .UNSPECIFIED., .F., .F.,
 ( 4, 2, 2, 2, 2, 2, 2, 2, 2, 1, 2, 2, 2, 2, 2, 2, 2, 2, 2, 2, 2, 2, 2, 2, 4 ),
 ( 6.997332055170240228E-20, 0.002296365050924792459, 0.003444547576387190207, 0.004592730101849587521, 0.006889095152774382148, 0.008037277678236776426, 0.009185460203699171572, 0.01148182525462396186, 0.01263000778008635874, 0.01377819030554875562, 0.01492637283101115250, 0.01607455535647354938, 0.01837092040739833967, 0.01951910293286073655, 0.02066728545832313343, 0.02296365050924792373, 0.02411183303471032408, 0.02526001556017272442, 0.02755638061109752512, 0.02985274566202231541, 0.03100092818748471230, 0.03214911071294710571, 0.03444547576387189253, 0.03559365828933428594, 0.03674184081479667241 ),
 .UNSPECIFIED. ) ;
#10865 = ADVANCED_FACE ( 'NONE', ( #6759 ), #9017, .T. ) ;
#10866 = AXIS2_PLACEMENT_3D ( 'NONE', #1283, #4275, #7350 ) ;
#10867 = CARTESIAN_POINT ( 'NONE',  ( -249.7763361845706527, 11.55065150977181787, -2.186104012435922339 ) ) ;
#10868 = CARTESIAN_POINT ( 'NONE',  ( -242.3038136696815457, -6.626013037286656804, -10.00479684789021917 ) ) ;
#10869 = DIRECTION ( 'NONE',  ( -0.000000000000000000, -1.000000000000000000, 0.000000000000000000 ) ) ;
#10870 = VERTEX_POINT ( 'NONE', #5822 ) ;
#10871 = ORIENTED_EDGE ( 'NONE', *, *, #2151, .F. ) ;
#10872 = PRODUCT_DEFINITION_FORMATION_WITH_SPECIFIED_SOURCE ( 'ANY', '', #4464, .NOT_KNOWN. ) ;
#10873 = CARTESIAN_POINT ( 'NONE',  ( -115.4648407704221995, 20.08915143316778895, 234.1947771724274787 ) ) ;
#10874 = DIRECTION ( 'NONE',  ( -0.000000000000000000, 1.000000000000000000, 0.000000000000000000 ) ) ;
#10875 = CARTESIAN_POINT ( 'NONE',  ( 130.9697226060475259, 20.55460285142580545, -226.7975291077671329 ) ) ;
#10876 = DIRECTION ( 'NONE',  ( 0.4503334343941690632, -0.7071067811865280328, 0.5451603414288133109 ) ) ;
#10877 = DIRECTION ( 'NONE',  ( 0.5000000000000071054, 0.000000000000000000, -0.8660254037844345998 ) ) ;
#10878 = CARTESIAN_POINT ( 'NONE',  ( -197.8197553893924976, 30.00000000000000000, -64.27553482998719403 ) ) ;
#10879 = LINE ( 'NONE', #1755, #1402 ) ;
#10880 = AXIS2_PLACEMENT_3D ( 'NONE', #9575, #3570, #648 ) ;
#10881 = LINE ( 'NONE', #8933, #7605 ) ;
#10882 = EDGE_CURVE ( 'NONE', #2804, #7040, #2416, .T. ) ;
#10883 = ORIENTED_EDGE ( 'NONE', *, *, #3426, .T. ) ;
#10884 = DIRECTION ( 'NONE',  ( 0.000000000000000000, 0.000000000000000000, 1.000000000000000000 ) ) ;
#10885 = VERTEX_POINT ( 'NONE', #5684 ) ;
#10886 = VERTEX_POINT ( 'NONE', #687 ) ;
#10887 = ADVANCED_FACE ( 'NONE', ( #12880 ), #1134, .F. ) ;
#10888 = VECTOR ( 'NONE', #2891, 1000.000000000000000 ) ;
#10889 = CARTESIAN_POINT ( 'NONE',  ( 240.0429366796232387, -2.111384149273799249, 2.791848677268702339 ) ) ;
#10890 = ORIENTED_EDGE ( 'NONE', *, *, #12261, .F. ) ;
#10891 = CARTESIAN_POINT ( 'NONE',  ( 229.9000000000000057, 4.420290228262880206, -4.087913195986883075 ) ) ;
#10892 = CONICAL_SURFACE ( 'NONE', #77, 6.500000000000005329, 0.7853981633974547183 ) ;
#10893 = CARTESIAN_POINT ( 'NONE',  ( -258.8746690728235080, 20.08915143284549387, 34.10614053596890471 ) ) ;
#10894 = DIRECTION ( 'NONE',  ( 0.000000000000000000, 1.000000000000000000, 0.000000000000000000 ) ) ;
#10895 =( LENGTH_UNIT ( ) NAMED_UNIT ( * ) SI_UNIT ( .MILLI., .METRE. ) );
#10896 = DIRECTION ( 'NONE',  ( 1.000000000000000000, 0.000000000000000000, 0.000000000000000000 ) ) ;
#10897 = ORIENTED_EDGE ( 'NONE', *, *, #7366, .T. ) ;
#10898 = DIRECTION ( 'NONE',  ( -0.000000000000000000, -1.000000000000000000, 0.000000000000000000 ) ) ;
#10899 = ORIENTED_EDGE ( 'NONE', *, *, #3204, .T. ) ;
#10900 = CARTESIAN_POINT ( 'NONE',  ( -238.9443119646329876, 1.049071724482780299, 11.70307552132215534 ) ) ;
#10901 = ORIENTED_EDGE ( 'NONE', *, *, #10184, .F. ) ;
#10902 = AXIS2_PLACEMENT_3D ( 'NONE', #1374, #9558, #5440 ) ;
#10903 = AXIS2_PLACEMENT_3D ( 'NONE', #6660, #11793, #2576 ) ;
#10904 = DIRECTION ( 'NONE',  ( -0.4503334343941556295, 0.7071067811865489050, -0.5451603414287969906 ) ) ;
#10905 = PRESENTATION_STYLE_ASSIGNMENT (( #4829 ) ) ;
#10906 = CYLINDRICAL_SURFACE ( 'NONE', #4449, 5.500000000000007994 ) ;
#10907 = CARTESIAN_POINT ( 'NONE',  ( -229.9961257339021188, 11.67486194030054847, -1.531634783006589950 ) ) ;
#10908 = CARTESIAN_POINT ( 'NONE',  ( 136.1890905123932214, -25.00000000000000000, -208.4551069784743333 ) ) ;
#10909 = PRODUCT_DEFINITION_SHAPE ( 'NONE', 'NONE',  #13157 ) ;
#10910 = CARTESIAN_POINT ( 'NONE',  ( -244.3545189506059216, -8.356296374751478240, 8.612604422907843116 ) ) ;
#10911 = CIRCLE ( 'NONE', #12194, 250.1999999999999602 ) ;
#10912 = CARTESIAN_POINT ( 'NONE',  ( -238.7553599115560132, 0.5384408835009459882, -11.98839505287317841 ) ) ;
#10913 = CONTEXT_DEPENDENT_SHAPE_REPRESENTATION ( #7281, #8813 ) ;
#10914 = ORIENTED_EDGE ( 'NONE', *, *, #1074, .F. ) ;
#10915 = DIRECTION ( 'NONE',  ( 0.000000000000000000, 0.000000000000000000, 1.000000000000000000 ) ) ;
#10916 = EDGE_CURVE ( 'NONE', #12887, #12366, #5170, .T. ) ;
#10917 = ORIENTED_EDGE ( 'NONE', *, *, #446, .T. ) ;
#10918 = ORIENTED_EDGE ( 'NONE', *, *, #6060, .F. ) ;
#10919 = CARTESIAN_POINT ( 'NONE',  ( -249.7544427812662775, -11.44486579096268386, -2.664765659934758002 ) ) ;
#10920 = VERTEX_POINT ( 'NONE', #11950 ) ;
#10921 = AXIS2_PLACEMENT_3D ( 'NONE', #4141, #2070, #812 ) ;
#10922 = AXIS2_PLACEMENT_3D ( 'NONE', #12832, #450, #4564 ) ;
#10923 = CARTESIAN_POINT ( 'NONE',  ( -196.8887528216966132, 20.55460285140358678, -172.6991790949711287 ) ) ;
#10924 = FACE_OUTER_BOUND ( 'NONE', #4697, .T. ) ;
#10925 = CARTESIAN_POINT ( 'NONE',  ( -27.68945685411286561, -30.00000000000000000, 290.6841825403027997 ) ) ;
#10926 = AXIS2_PLACEMENT_3D ( 'NONE', #4807, #6822, #2669 ) ;
#10927 = DIRECTION ( 'NONE',  ( 1.000000000000000000, 0.000000000000000000, 0.000000000000000000 ) ) ;
#10928 = CARTESIAN_POINT ( 'NONE',  ( -242.2626230870823463, 6.580656946580349498, 10.03470782660452976 ) ) ;
#10929 = CARTESIAN_POINT ( 'NONE',  ( -1.010328782420808020E-12, 20.79694577634649022, 260.7745447061710138 ) ) ;
#10930 = CARTESIAN_POINT ( 'NONE',  ( -34.28253040793653383, -138.4705547276867321, -24.00488622054099253 ) ) ;
#10931 = DIRECTION ( 'NONE',  ( 0.000000000000000000, 1.000000000000000000, 0.000000000000000000 ) ) ;
#10932 = ADVANCED_FACE ( 'NONE', ( #2800 ), #6625, .F. ) ;
#10933 = AXIS2_PLACEMENT_3D ( 'NONE', #12311, #6186, #11446 ) ;
#10934 = CONICAL_SURFACE ( 'NONE', #5834, 5.500000000000007994, 0.7853981633974461696 ) ;
#10935 = CARTESIAN_POINT ( 'NONE',  ( -249.2724874750445281, 10.50618518648595590, -5.261424415981784897 ) ) ;
#10936 =( REPRESENTATION_RELATIONSHIP ('NONE','NONE', #12019, #182 ) REPRESENTATION_RELATIONSHIP_WITH_TRANSFORMATION ( #8085 )SHAPE_REPRESENTATION_RELATIONSHIP( ) );
#10937 = CARTESIAN_POINT ( 'NONE',  ( -229.8947343418161893, -9.784924124804621925, -6.986540743649005236 ) ) ;
#10938 = VERTEX_POINT ( 'NONE', #12744 ) ;
#10939 = ORIENTED_EDGE ( 'NONE', *, *, #4505, .F. ) ;
#10940 = DIRECTION ( 'NONE',  ( 0.000000000000000000, 0.000000000000000000, 1.000000000000000000 ) ) ;
#10941 = DIRECTION ( 'NONE',  ( 0.000000000000000000, 0.000000000000000000, -1.000000000000000000 ) ) ;
#10942 = EDGE_CURVE ( 'NONE', #5825, #7844, #6888, .T. ) ;
#10943 = PRODUCT_DEFINITION_SHAPE ( 'NONE', 'NONE',  #13058 ) ;
#10944 = AXIS2_PLACEMENT_3D ( 'NONE', #6211, #8412, #12276 ) ;
#10945 = ADVANCED_FACE ( 'NONE', ( #9470 ), #8593, .F. ) ;
#10946 = CARTESIAN_POINT ( 'NONE',  ( -34.13493237016224668, 20.79694577639865471, 259.0935598599945138 ) ) ;
#10947 = DIRECTION ( 'NONE',  ( 0.000000000000000000, 0.7071067811865480168, 0.7071067811865470176 ) ) ;
#10948 = DIRECTION ( 'NONE',  ( 6.982962677686266711E-15, 0.000000000000000000, -1.000000000000000000 ) ) ;
#10949 = AXIS2_PLACEMENT_3D ( 'NONE', #12992, #3981, #8058 ) ;
#10950 = FACE_OUTER_BOUND ( 'NONE', #1651, .T. ) ;
#10951 = ORIENTED_EDGE ( 'NONE', *, *, #2151, .T. ) ;
#10952 =( REPRESENTATION_RELATIONSHIP ('NONE','NONE', #12019, #182 ) REPRESENTATION_RELATIONSHIP_WITH_TRANSFORMATION ( #10767 )SHAPE_REPRESENTATION_RELATIONSHIP( ) );
#10953 = DIRECTION ( 'NONE',  ( 0.000000000000000000, 0.000000000000000000, 1.000000000000000000 ) ) ;
#10954 = CIRCLE ( 'NONE', #12235, 3.000000000000002665 ) ;
#10955 = CIRCLE ( 'NONE', #1385, 6.500000000000005329 ) ;
#10956 = CARTESIAN_POINT ( 'NONE',  ( -239.8728793007195179, -2.114429120494187408, 11.81232487964174638 ) ) ;
#10957 = VERTEX_POINT ( 'NONE', #12598 ) ;
#10958 = EDGE_LOOP ( 'NONE', ( #6687, #1018 ) ) ;
#10959 = CARTESIAN_POINT ( 'NONE',  ( 240.1560849993302611, -2.274296953689764145, 2.660406300277259994 ) ) ;
#10960 = ORIENTED_EDGE ( 'NONE', *, *, #332, .T. ) ;
#10961 = ADVANCED_FACE ( 'NONE', ( #471 ), #1405, .F. ) ;
#10962 = DIRECTION ( 'NONE',  ( 0.5024607274629889764, -0.3950277506594149224, -0.7690814609430700610 ) ) ;
#10963 = EDGE_CURVE ( 'NONE', #3038, #7702, #4529, .T. ) ;
#10964 = DIRECTION ( 'NONE',  ( 0.000000000000000000, 0.000000000000000000, 1.000000000000000000 ) ) ;
#10965 = AXIS2_PLACEMENT_3D ( 'NONE', #8865, #7136, #5934 ) ;
#10966 = FACE_OUTER_BOUND ( 'NONE', #2662, .T. ) ;
#10967 =( LENGTH_UNIT ( ) NAMED_UNIT ( * ) SI_UNIT ( .MILLI., .METRE. ) );
#10968 = EDGE_CURVE ( 'NONE', #11921, #2672, #404, .T. ) ;
#10969 = EDGE_LOOP ( 'NONE', ( #4548, #10989, #4345, #531 ) ) ;
#10970 = CARTESIAN_POINT ( 'NONE',  ( -239.1225034092054500, -1.367596997490950539, 11.67014394435902958 ) ) ;
#10971 = ORIENTED_EDGE ( 'NONE', *, *, #12395, .T. ) ;
#10972 = CARTESIAN_POINT ( 'NONE',  ( -239.5361044668155159, 1.848645179572584896, 11.60366368868220022 ) ) ;
#10973 = ORIENTED_EDGE ( 'NONE', *, *, #4351, .F. ) ;
#10974 = CIRCLE ( 'NONE', #549, 260.1830065359515061 ) ;
#10975 = CARTESIAN_POINT ( 'NONE',  ( 240.2344515802417959, -2.410164965830901451, -2.538069655751040266 ) ) ;
#10976 = CARTESIAN_POINT ( 'NONE',  ( -185.9653539489998195, -18.00000000000000000, -225.1241593668329699 ) ) ;
#10977 = CARTESIAN_POINT ( 'NONE',  ( 0.000000000000000000, 19.00000000000000000, -195.0000000000000000 ) ) ;
#10978 = CARTESIAN_POINT ( 'NONE',  ( -229.9849491715392844, 11.45184952815656310, -2.657836336733081950 ) ) ;
#10979 = FACE_BOUND ( 'NONE', #551, .T. ) ;
#10980 = CARTESIAN_POINT ( 'NONE',  ( -243.2557941747326993, -7.548840531214802141, 9.332172165351044768 ) ) ;
#10981 = CARTESIAN_POINT ( 'NONE',  ( -172.0303573358521305, 20.79694577634646535, -196.1676464792608954 ) ) ;
#10982 = ITEM_DEFINED_TRANSFORMATION ( 'NONE', 'NONE', #4206,  #805 ) ;
#10983 = EDGE_LOOP ( 'NONE', ( #10444, #7624, #10548, #7685 ) ) ;
#10984 = CARTESIAN_POINT ( 'NONE',  ( -238.9324305500051651, -1.023275421966679311, -11.70536273065333965 ) ) ;
#10985 = AXIS2_PLACEMENT_3D ( 'NONE', #11271, #9011, #9074 ) ;
#10986 = ORIENTED_EDGE ( 'NONE', *, *, #2924, .T. ) ;
#10987 = ORIENTED_EDGE ( 'NONE', *, *, #7614, .F. ) ;
#10988 = CARTESIAN_POINT ( 'NONE',  ( -248.6772030005851093, -10.03733143289317908, -6.108624101512084792 ) ) ;
#10989 = ORIENTED_EDGE ( 'NONE', *, *, #6556, .T. ) ;
#10990 = CARTESIAN_POINT ( 'NONE',  ( -130.9697226053157237, 20.55460285097016282, -226.7975291069864738 ) ) ;
#10991 = DIRECTION ( 'NONE',  ( -0.6368676505102707219, 0.000000000000000000, -0.7709731485165535192 ) ) ;
#10992 = DIRECTION ( 'NONE',  ( -0.4503334343941556295, 0.7071067811865489050, -0.5451603414287969906 ) ) ;
#10993 = DIRECTION ( 'NONE',  ( 0.000000000000000000, 1.000000000000000000, 0.000000000000000000 ) ) ;
#10994 = CARTESIAN_POINT ( 'NONE',  ( -197.8197553893924976, 29.00000000000000000, -69.77553482998720824 ) ) ;
#10995 = DIRECTION ( 'NONE',  ( 0.000000000000000000, -1.000000000000000000, 0.000000000000000000 ) ) ;
#10996 = DIRECTION ( 'NONE',  ( -0.9659258262890699775, 0.000000000000000000, 0.2588190451025145777 ) ) ;
#10997 = CARTESIAN_POINT ( 'NONE',  ( -229.9810369278718554, -11.37375499241069754, 3.048046500125209501 ) ) ;
#10998 = DIRECTION ( 'NONE',  ( 0.000000000000000000, 0.000000000000000000, 1.000000000000000000 ) ) ;
#10999 = EDGE_LOOP ( 'NONE', ( #9167, #5155, #1597 ) ) ;
#11000 = ORIENTED_EDGE ( 'NONE', *, *, #8234, .F. ) ;
#11001 = CARTESIAN_POINT ( 'NONE',  ( -190.1049936773165996, -18.00000000000000000, -230.1354848321905706 ) ) ;
#11002 = ADVANCED_FACE ( 'NONE', ( #6538 ), #10659, .T. ) ;
#11003 = ADVANCED_FACE ( 'NONE', ( #10468 ), #9656, .F. ) ;
#11004 = CIRCLE ( 'NONE', #3758, 9.900000000000019895 ) ;
#11005 = LINE ( 'NONE', #11277, #6235 ) ;
#11006 = CARTESIAN_POINT ( 'NONE',  ( 0.000000000000000000, 20.00000000000000000, 0.000000000000000000 ) ) ;
#11007 = DIRECTION ( 'NONE',  ( 0.6427876096865458022, 0.000000000000000000, -0.7660444431189726844 ) ) ;
#11008 = CARTESIAN_POINT ( 'NONE',  ( -245.3907676188946994, -8.935007734252014444, 7.630737089623142566 ) ) ;
#11009 = CONTEXT_DEPENDENT_SHAPE_REPRESENTATION ( #11873, #7340 ) ;
#11010 = TOROIDAL_SURFACE ( 'NONE', #10801, 252.1999999999999886, 2.000000000000000000 ) ;
#11011 = ORIENTED_EDGE ( 'NONE', *, *, #4508, .T. ) ;
#11012 = PRODUCT_DEFINITION ( 'UNKNOWN', '', #7681, #4887 ) ;
#11013 = DIRECTION ( 'NONE',  ( 0.000000000000000000, 0.9998057603070480415, -0.01970892327970899874 ) ) ;
#11014 = CARTESIAN_POINT ( 'NONE',  ( -239.0755113761929920, -1.313873759170463673, 11.92786187197615000 ) ) ;
#11015 = ORIENTED_EDGE ( 'NONE', *, *, #5923, .T. ) ;
#11016 = ORIENTED_EDGE ( 'NONE', *, *, #7704, .F. ) ;
#11017 = PRODUCT_DEFINITION_CONTEXT ( 'detailed design', #1834, 'design' ) ;
#11018 = DIRECTION ( 'NONE',  ( -1.000000000000000000, 0.000000000000000000, 0.000000000000000000 ) ) ;
#11019 = ORIENTED_EDGE ( 'NONE', *, *, #3171, .T. ) ;
#11020 = PRODUCT_DEFINITION_SHAPE ( 'NONE', 'NONE',  #13139 ) ;
#11021 = CARTESIAN_POINT ( 'NONE',  ( -248.8121438751408334, 10.11580272837505667, 5.977715408700031929 ) ) ;
#11022 = CARTESIAN_POINT ( 'NONE',  ( -234.7354397754233446, 19.96883745989621417, -115.7315435906453871 ) ) ;
#11023 = CARTESIAN_POINT ( 'NONE',  ( 132.6365829178909621, -19.40000000000000213, -260.1259780660157048 ) ) ;
#11024 = DIRECTION ( 'NONE',  ( 0.000000000000000000, 0.000000000000000000, 1.000000000000000000 ) ) ;
#11025 = ORIENTED_EDGE ( 'NONE', *, *, #911, .T. ) ;
#11026 = CARTESIAN_POINT ( 'NONE',  ( -239.5361044668159991, -1.848645179572815156, 11.60366368868215758 ) ) ;
#11027 = EDGE_CURVE ( 'NONE', #10501, #1505, #3456, .T. ) ;
#11029 = VERTEX_POINT ( 'NONE', #7534 ) ;
#11028 = AXIS2_PLACEMENT_3D ( 'NONE', #3543, #10680, #4542 ) ;
#11030 = ADVANCED_FACE ( 'NONE', ( #8408 ), #9237, .F. ) ;
#11031 = CARTESIAN_POINT ( 'NONE',  ( -238.9571479212536076, 1.076402573844281951, 11.70061130409436778 ) ) ;
#11032 = ORIENTED_EDGE ( 'NONE', *, *, #816, .F. ) ;
#11033 = CARTESIAN_POINT ( 'NONE',  ( 239.7985776503645354, -1.848645179573700004, -2.971954070984049956 ) ) ;
#11034 = DIRECTION ( 'NONE',  ( 0.000000000000000000, -1.000000000000000000, 0.000000000000000000 ) ) ;
#11035 = CARTESIAN_POINT ( 'NONE',  ( -210.0000000000000000, 19.40000000000000213, 5.100000000000000533 ) ) ;
#11036 = CONICAL_SURFACE ( 'NONE', #5937, 5.500000000000005329, 0.7853981633974461696 ) ;
#11037 = AXIS2_PLACEMENT_3D ( 'NONE', #10309, #3105, #8390 ) ;
#11038 = CARTESIAN_POINT ( 'NONE',  ( -229.9803371157412641, 11.35915247731612254, -3.029940864557863378 ) ) ;
#11039 = CARTESIAN_POINT ( 'NONE',  ( 238.9743710777160857, 8.519355453646930632E-11, 3.499999942258626984 ) ) ;
#11040 = CARTESIAN_POINT ( 'NONE',  ( -244.8267157024196194, -8.641841620791439027, 8.325778331725320669 ) ) ;
#11041 =( REPRESENTATION_RELATIONSHIP ('NONE','NONE', #12019, #5191 ) REPRESENTATION_RELATIONSHIP_WITH_TRANSFORMATION ( #3395 )SHAPE_REPRESENTATION_RELATIONSHIP( ) );
#11042 = AXIS2_PLACEMENT_3D ( 'NONE', #11088, #6095, #2810 ) ;
#11043 = CARTESIAN_POINT ( 'NONE',  ( -239.4329164351061365, 1.762478857497947971, -11.86986396130624044 ) ) ;
#11044 = CONTEXT_DEPENDENT_SHAPE_REPRESENTATION ( #6605, #9373 ) ;
#11045 = ORIENTED_EDGE ( 'NONE', *, *, #12738, .F. ) ;
#11046 = AXIS2_PLACEMENT_3D ( 'NONE', #7656, #7593, #3724 ) ;
#11047 = CARTESIAN_POINT ( 'NONE',  ( 0.000000000000000000, -1.848645179579245124, -239.8169934640529846 ) ) ;
#11048 = ORIENTED_EDGE ( 'NONE', *, *, #4013, .T. ) ;
#11049 = ADVANCED_FACE ( 'NONE', ( #5403 ), #10934, .F. ) ;
#11050 = PRODUCT_DEFINITION_SHAPE ( 'NONE', 'NONE',  #13086 ) ;
#11051 = VERTEX_POINT ( 'NONE', #9587 ) ;
#11052 = VECTOR ( 'NONE', #3493, 1000.000000000000000 ) ;
#11053 = CARTESIAN_POINT ( 'NONE',  ( -248.9237871404848761, -10.19078078235692431, 5.849051583267943499 ) ) ;
#11054 = VERTEX_POINT ( 'NONE', #12720 ) ;
#11055 = CARTESIAN_POINT ( 'NONE',  ( 226.7975291075301811, 20.55460285098495277, 130.9697226058104036 ) ) ;
#11056 = CARTESIAN_POINT ( 'NONE',  ( -246.4205552523959852, 9.380328320921323737, -7.484021896315862676 ) ) ;
#11057 = AXIS2_PLACEMENT_3D ( 'NONE', #6090, #9147, #12283 ) ;
#11058 = DIRECTION ( 'NONE',  ( 1.000000000000000000, 0.000000000000000000, 0.000000000000000000 ) ) ;
#11059 = CARTESIAN_POINT ( 'NONE',  ( 11.00000000000000000, 0.000000000000000000, 250.0000000000000000 ) ) ;
#11060 = CARTESIAN_POINT ( 'NONE',  ( -244.7967862073442120, 8.624712650776588774, 8.343521798077146556 ) ) ;
#11061 = AXIS2_PLACEMENT_3D ( 'NONE', #7308, #5496, #10362 ) ;
#11062 = CYLINDRICAL_SURFACE ( 'NONE', #7900, 249.7999999999999829 ) ;
#11063 = CARTESIAN_POINT ( 'NONE',  ( 36.24423871767953642, -138.4705547276867321, 20.92562098022590433 ) ) ;
#11064 = CARTESIAN_POINT ( 'NONE',  ( 235.0999999999999943, 2.749465840844381948, -0.05419953901919974393 ) ) ;
#11065 = AXIS2_PLACEMENT_3D ( 'NONE', #9697, #1782, #8844 ) ;
#11066 = ITEM_DEFINED_TRANSFORMATION ( 'NONE', 'NONE', #7464,  #805 ) ;
#11067 = DIRECTION ( 'NONE',  ( 0.6368676505102707219, 0.000000000000000000, 0.7709731485165535192 ) ) ;
#11068 = ORIENTED_EDGE ( 'NONE', *, *, #4013, .F. ) ;
#11069 = VERTEX_POINT ( 'NONE', #4518 ) ;
#11070 = AXIS2_PLACEMENT_3D ( 'NONE', #11059, #4987, #1930 ) ;
#11071 = DIRECTION ( 'NONE',  ( -0.6368676505102707219, 0.000000000000000000, -0.7709731485165536302 ) ) ;
#11072 = CARTESIAN_POINT ( 'NONE',  ( 3.010181832304193602E-14, 22.00000000000000000, 245.7999999999999829 ) ) ;
#11073 = LINE ( 'NONE', #1569, #1273 ) ;
#11074 = CARTESIAN_POINT ( 'NONE',  ( 226.3083638779000069, 20.79694577591247295, -130.6873781523096056 ) ) ;
#11075 = CARTESIAN_POINT ( 'NONE',  ( -197.8197553893909912, 30.00000000000000000, 58.77553482999130807 ) ) ;
#11076 =( BOUNDED_SURFACE ( )  B_SPLINE_SURFACE ( 3, 3, ( 
 ( #3739, #10008, #4935, #11877, #6816, #10873, #5813, #8277, #145, #10131, #4134, #1269, #4067, #6208, #6339, #10194, #11270, #10328, #2132, #12272, #5059, #10261, #5196, #10391, #6079, #9273, #4195, #1138, #8145, #12339, #11201, #12465, #12210, #2261, #3061, #3188, #12404, #1068, #5126, #7335, #8216, #2066, #11405, #9203, #2006, #80, #6139, #205, #7143, #7272, #3256, #8406, #5332, #9136, #7397, #3320, #9402, #269, #6277, #4327, #3122, #7201, #11336, #2200, #1205, #5264 ),
 ( #9334, #1003, #11, #4262, #8343, #9522, #10466, #11466, #9654, #10531, #4645, #12661, #3650, #1598, #11732, #3453, #2524, #6602, #3523, #4516, #1334, #4452, #536, #10657, #9712, #7592, #1463, #469, #2460, #12786, #7532, #11605, #8728, #11669, #1529, #5660, #2330, #594, #6475, #12528, #3587, #4584, #6406, #8537, #8660, #5594, #5401, #12718, #5527, #8601, #6536, #9468, #10589, #9585, #341, #7655, #2585, #4389, #8471, #3385, #1403, #7467, #6671, #10728, #11540, #12596 ),
 ( #2395, #5462, #402, #5928, #11858, #2648, #4712, #9992, #9855, #1798, #5561, #12857, #12055, #2843, #1728, #860, #664, #7722, #11997, #7995, #12990, #735, #9783, #1658, #10923, #6736, #11804, #10990, #2906, #10787, #3921, #8860, #3782, #4919, #4984, #1862, #6930, #8927, #6863, #11925, #12921, #5725, #8994, #9058, #2774, #3852, #7855, #4850, #8792, #5864, #6798, #10854, #3723, #7789, #11055, #4784, #2707, #6991, #1926, #9923, #794, #7921, #11306, #5997, #5794, #10055 ),
 ( #929, #12388, #8263, #4250, #7129, #2052, #3045, #4120, #12324, #11185, #1194, #8057, #8200, #5113, #8330, #7060, #12260, #5250, #6122, #2978, #3980, #2185, #10177, #10377, #5180, #9389, #7324, #3242, #9190, #3176, #7257, #9259, #10247, #11119, #990, #1991, #67, #6064, #10315, #11393, #1054, #2253, #3110, #7187, #11253, #2116, #193, #6327, #4051, #9320, #1254, #132, #6266, #8131, #12122, #5043, #5319, #6193, #1123, #10117, #9119, #202, #11322, #4182, #12191, #10929 ) ),
 .UNSPECIFIED., .F., .T., .F. ) 
 B_SPLINE_SURFACE_WITH_KNOTS ( ( 4, 4 ),
 ( 4, 2, 2, 2, 2, 2, 2, 2, 2, 2, 2, 2, 2, 2, 2, 2, 2, 2, 2, 2, 2, 2, 2, 2, 2, 2, 2, 2, 2, 2, 2, 2, 4 ),
 ( 0.000000000000000000, 1.000000000000000000 ),
 ( 0.5000000000000000000, 0.5312500000000000000, 0.5625000000000000000, 0.5937500000000000000, 0.6250000000000000000, 0.6562500000000000000, 0.6875000000000000000, 0.7187500000000000000, 0.7500000000000000000, 0.7812500000000000000, 0.8125000000000000000, 0.8437500000000000000, 0.8750000000000000000, 0.9062500000000000000, 0.9375000000000000000, 0.9687500000000000000, 1.000000000000000000, 1.031250000000000000, 1.062500000000000000, 1.093750000000000000, 1.125000000000000000, 1.156250000000000000, 1.187500000000000000, 1.218750000000000000, 1.250000000000000000, 1.281250000000000000, 1.312500000000000000, 1.343750000000000000, 1.375000000000000000, 1.406250000000000000, 1.437500000000000000, 1.468750000000000000, 1.500000000000000000 ),
 .UNSPECIFIED. ) 
 GEOMETRIC_REPRESENTATION_ITEM ( )  RATIONAL_B_SPLINE_SURFACE ( (
 ( 1.000000000000000000, 1.000000000000000000, 1.000000000000000000, 1.000000000000000000, 1.000000000000000000, 1.000000000000000000, 1.000000000000000000, 1.000000000000000000, 1.000000000000000000, 1.000000000000000000, 1.000000000000000000, 1.000000000000000000, 1.000000000000000000, 1.000000000000000000, 1.000000000000000000, 1.000000000000000000, 1.000000000000000000, 1.000000000000000000, 1.000000000000000000, 1.000000000000000000, 1.000000000000000000, 1.000000000000000000, 1.000000000000000000, 1.000000000000000000, 1.000000000000000000, 1.000000000000000000, 1.000000000000000000, 1.000000000000000000, 1.000000000000000000, 1.000000000000000000, 1.000000000000000000, 1.000000000000000000, 1.000000000000000000, 1.000000000000000000, 1.000000000000000000, 1.000000000000000000, 1.000000000000000000, 1.000000000000000000, 1.000000000000000000, 1.000000000000000000, 1.000000000000000000, 1.000000000000000000, 1.000000000000000000, 1.000000000000000000, 1.000000000000000000, 1.000000000000000000, 1.000000000000000000, 1.000000000000000000, 1.000000000000000000, 1.000000000000000000, 1.000000000000000000, 1.000000000000000000, 1.000000000000000000, 1.000000000000000000, 1.000000000000000000, 1.000000000000000000, 1.000000000000000000, 1.000000000000000000, 1.000000000000000000, 1.000000000000000000, 1.000000000000000000, 1.000000000000000000, 1.000000000000000000, 1.000000000000000000, 1.000000000000000000, 1.000000000000000000),
 ( 0.4027746460044325238, 0.4027746460044325238, 0.4027746460044540067, 0.4027746460044540067, 0.4027746460044225318, 0.4027746460044225318, 0.4027746460043825083, 0.4027746460043825083, 0.4027746460043430399, 0.4027746460043430399, 0.4027746460043289956, 0.4027746460043289956, 0.4027746460043410415, 0.4027746460043410415, 0.4027746460044525079, 0.4027746460044525079, 0.4027746460044325238, 0.4027746460044325238, 0.4027746460044525079, 0.4027746460044525079, 0.4027746460043595267, 0.4027746460043595267, 0.4027746460044215326, 0.4027746460044215326, 0.4027746460043590271, 0.4027746460043590271, 0.4027746460044335230, 0.4027746460044335230, 0.4027746460043410415, 0.4027746460043410415, 0.4027746460042145316, 0.4027746460042145316, 0.4027746460044325238, 0.4027746460044325238, 0.4027746460044535071, 0.4027746460044535071, 0.4027746460044230314, 0.4027746460044230314, 0.4027746460043575283, 0.4027746460043575283, 0.4027746460043590271, 0.4027746460043590271, 0.4027746460043944987, 0.4027746460043944987, 0.4027746460043630239, 0.4027746460043630239, 0.4027746460044520083, 0.4027746460044520083, 0.4027746460044325238, 0.4027746460044325238, 0.4027746460044530075, 0.4027746460044530075, 0.4027746460043180043, 0.4027746460043180043, 0.4027746460043225007, 0.4027746460043225007, 0.4027746460043230003, 0.4027746460043230003, 0.4027746460043944987, 0.4027746460043944987, 0.4027746460042090360, 0.4027746460042090360, 0.4027746460044520083, 0.4027746460044520083, 0.4027746460044325238, 0.4027746460044325238),
 ( 0.4027746460044325238, 0.4027746460044325238, 0.4027746460044540067, 0.4027746460044540067, 0.4027746460044225318, 0.4027746460044225318, 0.4027746460043825083, 0.4027746460043825083, 0.4027746460043430399, 0.4027746460043430399, 0.4027746460043289956, 0.4027746460043289956, 0.4027746460043410415, 0.4027746460043410415, 0.4027746460044525079, 0.4027746460044525079, 0.4027746460044325238, 0.4027746460044325238, 0.4027746460044525079, 0.4027746460044525079, 0.4027746460043595267, 0.4027746460043595267, 0.4027746460044215326, 0.4027746460044215326, 0.4027746460043590271, 0.4027746460043590271, 0.4027746460044335230, 0.4027746460044335230, 0.4027746460043410415, 0.4027746460043410415, 0.4027746460042145316, 0.4027746460042145316, 0.4027746460044325238, 0.4027746460044325238, 0.4027746460044535071, 0.4027746460044535071, 0.4027746460044230314, 0.4027746460044230314, 0.4027746460043575283, 0.4027746460043575283, 0.4027746460043590271, 0.4027746460043590271, 0.4027746460043944987, 0.4027746460043944987, 0.4027746460043630239, 0.4027746460043630239, 0.4027746460044520083, 0.4027746460044520083, 0.4027746460044325238, 0.4027746460044325238, 0.4027746460044530075, 0.4027746460044530075, 0.4027746460043180043, 0.4027746460043180043, 0.4027746460043225007, 0.4027746460043225007, 0.4027746460043230003, 0.4027746460043230003, 0.4027746460043944987, 0.4027746460043944987, 0.4027746460042090360, 0.4027746460042090360, 0.4027746460044520083, 0.4027746460044520083, 0.4027746460044325238, 0.4027746460044325238),
 ( 1.000000000000000000, 1.000000000000000000, 1.000000000000000000, 1.000000000000000000, 1.000000000000000000, 1.000000000000000000, 1.000000000000000000, 1.000000000000000000, 1.000000000000000000, 1.000000000000000000, 1.000000000000000000, 1.000000000000000000, 1.000000000000000000, 1.000000000000000000, 1.000000000000000000, 1.000000000000000000, 1.000000000000000000, 1.000000000000000000, 1.000000000000000000, 1.000000000000000000, 1.000000000000000000, 1.000000000000000000, 1.000000000000000000, 1.000000000000000000, 1.000000000000000000, 1.000000000000000000, 1.000000000000000000, 1.000000000000000000, 1.000000000000000000, 1.000000000000000000, 1.000000000000000000, 1.000000000000000000, 1.000000000000000000, 1.000000000000000000, 1.000000000000000000, 1.000000000000000000, 1.000000000000000000, 1.000000000000000000, 1.000000000000000000, 1.000000000000000000, 1.000000000000000000, 1.000000000000000000, 1.000000000000000000, 1.000000000000000000, 1.000000000000000000, 1.000000000000000000, 1.000000000000000000, 1.000000000000000000, 1.000000000000000000, 1.000000000000000000, 1.000000000000000000, 1.000000000000000000, 1.000000000000000000, 1.000000000000000000, 1.000000000000000000, 1.000000000000000000, 1.000000000000000000, 1.000000000000000000, 1.000000000000000000, 1.000000000000000000, 1.000000000000000000, 1.000000000000000000, 1.000000000000000000, 1.000000000000000000, 1.000000000000000000, 1.000000000000000000) ) ) 
 REPRESENTATION_ITEM ( '' )  SURFACE ( )  );
#11077 = DIRECTION ( 'NONE',  ( -0.7071067811865413555, 0.000000000000000000, -0.7071067811865536790 ) ) ;
#11078 = CIRCLE ( 'NONE', #10226, 4.500000000000000000 ) ;
#11079 = DIRECTION ( 'NONE',  ( 1.125045280045195686E-16, -0.3950277506594045973, 0.9186691875800402363 ) ) ;
#11080 = ORIENTED_EDGE ( 'NONE', *, *, #6699, .T. ) ;
#11081 = ADVANCED_FACE ( 'NONE', ( #5596 ), #88, .F. ) ;
#11082 = DIRECTION ( 'NONE',  ( 0.000000000000000000, 1.000000000000000000, 0.000000000000000000 ) ) ;
#11083 = ADVANCED_FACE ( 'NONE', ( #11734, #11543 ), #6673, .F. ) ;
#11084 = AXIS2_PLACEMENT_3D ( 'NONE', #138, #4188, #6271 ) ;
#11085 = CARTESIAN_POINT ( 'NONE',  ( -239.4443750393931509, -1.773851958419369712, 11.86816533821130015 ) ) ;
#11086 = ORIENTED_EDGE ( 'NONE', *, *, #11781, .F. ) ;
#11087 = ORIENTED_EDGE ( 'NONE', *, *, #8511, .F. ) ;
#11088 = CARTESIAN_POINT ( 'NONE',  ( 0.000000000000000000, -25.00000000000000000, 0.000000000000000000 ) ) ;
#11089 = CARTESIAN_POINT ( 'NONE',  ( -185.9653539489998195, -19.00000000000000000, -225.1241593668329699 ) ) ;
#11090 = CARTESIAN_POINT ( 'NONE',  ( -249.6587182941822221, 11.13358978266949961, 3.756204109565398852 ) ) ;
#11091 = CARTESIAN_POINT ( 'NONE',  ( 17.05314194195614874, 20.08915143307225648, 260.5542428346390125 ) ) ;
#11092 = DIRECTION ( 'NONE',  ( -0.000000000000000000, -1.000000000000000000, 0.000000000000000000 ) ) ;
#11093 = CARTESIAN_POINT ( 'NONE',  ( -238.8364110056832885, -0.8171106957274414384, -11.97229870871749746 ) ) ;
#11094 = CARTESIAN_POINT ( 'NONE',  ( -245.4195491717965751, 8.949151682147107323, 7.614144253907443094 ) ) ;
#11095 = ORIENTED_EDGE ( 'NONE', *, *, #11459, .F. ) ;
#11096 = CARTESIAN_POINT ( 'NONE',  ( -239.0623374290204595, -1.272322106364155214, 11.68094603905051088 ) ) ;
#11098 = VERTEX_POINT ( 'NONE', #271 ) ;
#11097 = AXIS2_PLACEMENT_3D ( 'NONE', #9041, #174, #12102 ) ;
#11099 = CARTESIAN_POINT ( 'NONE',  ( -238.7109915808064500, 2.244475480116206709E-14, 11.74999999995203126 ) ) ;
#11100 = ORIENTED_EDGE ( 'NONE', *, *, #1899, .F. ) ;
#11101 = CIRCLE ( 'NONE', #2154, 6.500000000000005329 ) ;
#11102 = CARTESIAN_POINT ( 'NONE',  ( -248.5207756042016172, 9.904443212642727090, -6.775263356373602441 ) ) ;
#11103 = FACE_OUTER_BOUND ( 'NONE', #2773, .T. ) ;
#11104 = LINE ( 'NONE', #9970, #5560 ) ;
#11105 = CARTESIAN_POINT ( 'NONE',  ( 238.9743710777160857, 8.519355453646930632E-11, 3.499999942258626984 ) ) ;
#11106 = ADVANCED_FACE ( 'NONE', ( #9404 ), #4329, .F. ) ;
#11107 = CARTESIAN_POINT ( 'NONE',  ( 0.000000000000000000, 24.99999999999995737, 0.000000000000000000 ) ) ;
#11108 = EDGE_CURVE ( 'NONE', #1185, #6448, #11468, .T. ) ;
#11109 = DIRECTION ( 'NONE',  ( -0.000000000000000000, -1.000000000000000000, 0.000000000000000000 ) ) ;
#11110 = CARTESIAN_POINT ( 'NONE',  ( 0.000000000000000000, 19.00000000000000000, -213.5000000000000000 ) ) ;
#11111 = CARTESIAN_POINT ( 'NONE',  ( -238.6985546646470198, 6.516754929249349828E-09, -12.00000000011316459 ) ) ;
#11112 = ORIENTED_EDGE ( 'NONE', *, *, #5494, .T. ) ;
#11113 = CARTESIAN_POINT ( 'NONE',  ( -238.7322540142980927, -0.3343210646034411870, -11.74538300442941541 ) ) ;
#11114 = VECTOR ( 'NONE', #7663, 1000.000000000000000 ) ;
#11115 = CARTESIAN_POINT ( 'NONE',  ( -245.0843090350436171, -8.789319852992315774, -8.173033111772259218 ) ) ;
#11116 = CARTESIAN_POINT ( 'NONE',  ( -249.6893775633026848, -11.21617121157748542, 3.501676138744457933 ) ) ;
#11117 = ORIENTED_EDGE ( 'NONE', *, *, #8577, .F. ) ;
#11118 = CIRCLE ( 'NONE', #12398, 6.500000000000005329 ) ;
#11119 = CARTESIAN_POINT ( 'NONE',  ( 17.06760680800665142, 20.79694577634646180, -260.7745447061710138 ) ) ;
#11120 = DIRECTION ( 'NONE',  ( 0.000000000000000000, -1.000000000000000000, 0.000000000000000000 ) ) ;
#11121 = DIRECTION ( 'NONE',  ( -1.000000000000000000, 0.000000000000000000, 0.000000000000000000 ) ) ;
#11122 = CIRCLE ( 'NONE', #8152, 6.499999999999999112 ) ;
#11123 = CARTESIAN_POINT ( 'NONE',  ( -241.3731105455979389, -5.422910281729395265, -10.42375653607661334 ) ) ;
#11124 = EDGE_CURVE ( 'NONE', #7072, #12496, #5930, .T. ) ;
#11125 = CARTESIAN_POINT ( 'NONE',  ( -249.7999494874249251, 11.99892863384215325, 1.190337990169640703 ) ) ;
#11126 =( REPRESENTATION_RELATIONSHIP ('NONE','NONE', #12019, #5191 ) REPRESENTATION_RELATIONSHIP_WITH_TRANSFORMATION ( #11742 )SHAPE_REPRESENTATION_RELATIONSHIP( ) );
#11127 = FILL_AREA_STYLE ('',( #11931 ) ) ;
#11128 = CARTESIAN_POINT ( 'NONE',  ( 24.00488622054042054, -138.4705547276867321, 34.28253040793692463 ) ) ;
#11129 = CYLINDRICAL_SURFACE ( 'NONE', #4357, 5.499999999999986677 ) ;
#11130 = ADVANCED_FACE ( 'NONE', ( #12923 ), #10399, .F. ) ;
#11131 = PRODUCT_DEFINITION_SHAPE ( 'NONE', 'NONE',  #13136 ) ;
#11132 = AXIS2_PLACEMENT_3D ( 'NONE', #3068, #7079, #10202 ) ;
#11133 = DIRECTION ( 'NONE',  ( 0.000000000000000000, 0.9998057603070480415, -0.01970892327970899874 ) ) ;
#11134 = CONICAL_SURFACE ( 'NONE', #5393, 251.1999999999999886, 0.7853981633974207455 ) ;
#11135 = EDGE_LOOP ( 'NONE', ( #5572, #7815, #8276, #7939, #7412, #2920 ) ) ;
#11136 = VERTEX_POINT ( 'NONE', #9995 ) ;
#11137 = CARTESIAN_POINT ( 'NONE',  ( 71.82423009839129691, 30.00000000000000000, 190.8354503650404865 ) ) ;
#11138 = CYLINDRICAL_SURFACE ( 'NONE', #7209, 5.500000000000005329 ) ;
#11139 = LINE ( 'NONE', #7693, #8722 ) ;
#11140 = VECTOR ( 'NONE', #4752, 1000.000000000000114 ) ;
#11141 = CARTESIAN_POINT ( 'NONE',  ( 239.7985776503625175, 1.848645179571945185, -2.971954070985139751 ) ) ;
#11142 = AXIS2_PLACEMENT_3D ( 'NONE', #1381, #1115, #7444 ) ;
#11143 = CARTESIAN_POINT ( 'NONE',  ( 27.68945685411497593, -30.00000000000000000, -290.6841825403026291 ) ) ;
#11144 = CARTESIAN_POINT ( 'NONE',  ( 0.000000000000000000, 0.000000000000000000, 0.000000000000000000 ) ) ;
#11145 = AXIS2_PLACEMENT_3D ( 'NONE', #5286, #11427, #494 ) ;
#11146 = CARTESIAN_POINT ( 'NONE',  ( -241.2291919110257368, -5.202024195681614671, 10.53597307945316963 ) ) ;
#11147 = ORIENTED_EDGE ( 'NONE', *, *, #2555, .F. ) ;
#11148 = FACE_BOUND ( 'NONE', #10356, .T. ) ;
#11149 = CARTESIAN_POINT ( 'NONE',  ( 229.9737165936600718, -0.4586479115007087159, 3.477305464001514412 ) ) ;
#11150 = VERTEX_POINT ( 'NONE', #737 ) ;
#11151 = EDGE_LOOP ( 'NONE', ( #7051, #12067, #1595, #4609 ) ) ;
#11152 = DIRECTION ( 'NONE',  ( 0.000000000000000000, 1.000000000000000000, 0.000000000000000000 ) ) ;
#11153 = CARTESIAN_POINT ( 'NONE',  ( 294.1869546181097235, -30.00000000000000000, 31.92980917095290749 ) ) ;
#11154 = CONICAL_SURFACE ( 'NONE', #7117, 5.500000000000005329, 0.7853981633974461696 ) ;
#11155 = CARTESIAN_POINT ( 'NONE',  ( -248.2181897916257185, 9.855491095746206298, 6.397958699693558238 ) ) ;
#11156 = SHAPE_REPRESENTATION ( 'Internal Mounting Flange Ring', ( #805 ), #1235 ) ;
#11157 = EDGE_CURVE ( 'NONE', #1858, #8515, #12859, .T. ) ;
#11158 = CARTESIAN_POINT ( 'NONE',  ( -261.1558126970361400, 19.96883746053716990, -17.09264059830048410 ) ) ;
#11159 = CARTESIAN_POINT ( 'NONE',  ( -239.2610567797048304, -1.576377190171931453, -11.89622111457706133 ) ) ;
#11160 = CARTESIAN_POINT ( 'NONE',  ( -243.1833766791151277, 7.470616520408806416, 9.069320236312849559 ) ) ;
#11162 = ORIENTED_EDGE ( 'NONE', *, *, #5981, .T. ) ;
#11161 = AXIS2_PLACEMENT_3D ( 'NONE', #8661, #5662, #5114 ) ;
#11163 = CARTESIAN_POINT ( 'NONE',  ( 8.533827019709789852, 20.79694577634646180, 260.7745447061712412 ) ) ;
#11164 = ORIENTED_EDGE ( 'NONE', *, *, #10595, .T. ) ;
#11165 = CARTESIAN_POINT ( 'NONE',  ( 0.000000000000000000, 0.000000000000000000, 0.000000000000000000 ) ) ;
#11166 = EDGE_LOOP ( 'NONE', ( #6259, #1155, #9420, #11702 ) ) ;
#11167 = AXIS2_PLACEMENT_3D ( 'NONE', #463, #588, #1592 ) ;
#11168 = FACE_OUTER_BOUND ( 'NONE', #7700, .T. ) ;
#11169 = CARTESIAN_POINT ( 'NONE',  ( 240.1881190900947445, 2.326983775934756693, 2.614448608538753938 ) ) ;
#11170 = CARTESIAN_POINT ( 'NONE',  ( 0.000000000000000000, 22.00000000000000000, 0.000000000000000000 ) ) ;
#11171 = EDGE_CURVE ( 'NONE', #11299, #5825, #2650, .T. ) ;
#11172 = EDGE_CURVE ( 'NONE', #8752, #5508, #5797, .T. ) ;
#11173 = CYLINDRICAL_SURFACE ( 'NONE', #9417, 3.000000000000000000 ) ;
#11174 = CARTESIAN_POINT ( 'NONE',  ( 3.066299324940445530E-14, 21.99999999999995381, 250.3823410207189966 ) ) ;
#11175 = CARTESIAN_POINT ( 'NONE',  ( -239.9450917581429792, -2.156506209390995021, 11.80463811257499884 ) ) ;
#11176 = CARTESIAN_POINT ( 'NONE',  ( -17.06764083276507904, 20.79694577634647601, 260.3553053170168141 ) ) ;
#11177 = ORIENTED_EDGE ( 'NONE', *, *, #5225, .F. ) ;
#11178 = CARTESIAN_POINT ( 'NONE',  ( -239.0839813682398187, -1.310043317831860010, -11.67696021831089759 ) ) ;
#11179 = ORIENTED_EDGE ( 'NONE', *, *, #6959, .F. ) ;
#11180 = CARTESIAN_POINT ( 'NONE',  ( -249.6782235448949905, 11.18495322599711450, -3.599910145184412436 ) ) ;
#11181 = CARTESIAN_POINT ( 'NONE',  ( -122.2593324768321992, 19.00000000000000000, 173.7755348299905052 ) ) ;
#11182 = EDGE_CURVE ( 'NONE', #9146, #1858, #12736, .T. ) ;
#11183 = CARTESIAN_POINT ( 'NONE',  ( -249.6782235448939389, -11.18495322599737740, 3.599910145183604193 ) ) ;
#11184 = VERTEX_POINT ( 'NONE', #7858 ) ;
#11185 = CARTESIAN_POINT ( 'NONE',  ( -196.4640694352650030, 20.79694577634417030, 172.3268284098779759 ) ) ;
#11186 = CARTESIAN_POINT ( 'NONE',  ( -246.3576883201962175, 9.357104192357786232, -7.512982112911617882 ) ) ;
#11187 = DIRECTION ( 'NONE',  ( 1.000000000000000000, 0.000000000000000000, 0.000000000000000000 ) ) ;
#11188 = CARTESIAN_POINT ( 'NONE',  ( -246.7375545308477456, -9.485935069199962655, -6.933947691877577313 ) ) ;
#11189 = CONICAL_SURFACE ( 'NONE', #8430, 250.1999999999999602, 0.7853981633975041232 ) ;
#11190 =( REPRESENTATION_RELATIONSHIP ('NONE','NONE', #12019, #182 ) REPRESENTATION_RELATIONSHIP_WITH_TRANSFORMATION ( #1440 )SHAPE_REPRESENTATION_RELATIONSHIP( ) );
#11191 = CARTESIAN_POINT ( 'NONE',  ( -249.7969288063768545, 11.93744875557469953, -1.454679372240188506 ) ) ;
#11192 = DIRECTION ( 'NONE',  ( 0.000000000000000000, -1.000000000000000000, 0.000000000000000000 ) ) ;
#11193 = DIRECTION ( 'NONE',  ( 0.3518698652246288749, 0.5538822189107470706, 0.7545873610930072806 ) ) ;
#11194 = CARTESIAN_POINT ( 'NONE',  ( -229.7006282228656744, -0.7680959398531020943, 11.73127646695761506 ) ) ;
#11195 = CONTEXT_DEPENDENT_SHAPE_REPRESENTATION ( #8180, #2798 ) ;
#11196 = EDGE_CURVE ( 'NONE', #2438, #12027, #8499, .T. ) ;
#11197 = ADVANCED_FACE ( 'NONE', ( #10790 ), #8931, .F. ) ;
#11198 = DIRECTION ( 'NONE',  ( 0.000000000000000000, 1.000000000000000000, 0.000000000000000000 ) ) ;
#11199 = VERTEX_POINT ( 'NONE', #2776 ) ;
#11200 = ORIENTED_EDGE ( 'NONE', *, *, #7597, .F. ) ;
#11201 = CARTESIAN_POINT ( 'NONE',  ( -67.55708173894439028, 20.08915143292001204, -252.2208631666825056 ) ) ;
#11202 = CARTESIAN_POINT ( 'NONE',  ( 0.000000000000000000, 2.772967769359004908, 0.000000000000000000 ) ) ;
#11203 = ADVANCED_FACE ( 'NONE', ( #12993 ), #3854, .F. ) ;
#11204 = CARTESIAN_POINT ( 'NONE',  ( 71.82423009839129691, 30.00000000000000000, 190.8354503650404865 ) ) ;
#11205 = DIRECTION ( 'NONE',  ( 0.000000000000000000, 0.000000000000000000, 1.000000000000000000 ) ) ;
#11206 = DIRECTION ( 'NONE',  ( 0.6368676505102696117, 0.000000000000000000, 0.7709731485165545184 ) ) ;
#11207 = DIRECTION ( 'NONE',  ( 0.08715574274766850482, 0.000000000000000000, -0.9961946980917446570 ) ) ;
#11208 = CARTESIAN_POINT ( 'NONE',  ( -244.0310755556703270, -8.130894646083811850, 8.482269560327180713 ) ) ;
#11209 = ITEM_DEFINED_TRANSFORMATION ( 'NONE', 'NONE', #3358,  #805 ) ;
#11210 = ORIENTED_EDGE ( 'NONE', *, *, #4437, .T. ) ;
#11211 = FACE_OUTER_BOUND ( 'NONE', #7682, .T. ) ;
#11212 = EDGE_CURVE ( 'NONE', #4889, #3851, #8698, .T. ) ;
#11213 = DIRECTION ( 'NONE',  ( 0.000000000000000000, 0.000000000000000000, -1.000000000000000000 ) ) ;
#11214 = ORIENTED_EDGE ( 'NONE', *, *, #355, .F. ) ;
#11215 = ORIENTED_EDGE ( 'NONE', *, *, #8183, .T. ) ;
#11216 = PRODUCT_DEFINITION_SHAPE ( 'NONE', 'NONE',  #13098 ) ;
#11217 = LINE ( 'NONE', #7355, #7207 ) ;
#11218 = DIRECTION ( 'NONE',  ( 0.6368676505102698338, 0.000000000000000000, 0.7709731485165541853 ) ) ;
#11219 = VECTOR ( 'NONE', #2725, 1000.000000000000000 ) ;
#11220 = CARTESIAN_POINT ( 'NONE',  ( -67.71318189681706201, 19.96883746180772690, 252.8031682256479655 ) ) ;
#11221 = DIRECTION ( 'NONE',  ( -0.000000000000000000, -1.000000000000000000, 0.000000000000000000 ) ) ;
#11222 = CARTESIAN_POINT ( 'NONE',  ( 0.000000000000000000, 0.000000000000000000, 0.000000000000000000 ) ) ;
#11223 = CARTESIAN_POINT ( 'NONE',  ( -241.6806182397082807, 5.858727364634749968, 10.18566440554176289 ) ) ;
#11224 = ORIENTED_EDGE ( 'NONE', *, *, #6081, .F. ) ;
#11225 = CARTESIAN_POINT ( 'NONE',  ( 34.05310945291965652, 20.79694577634646180, 258.6823826759384133 ) ) ;
#11226 = EDGE_LOOP ( 'NONE', ( #11296, #838, #5172, #4025 ) ) ;
#11227 = CARTESIAN_POINT ( 'NONE',  ( 0.000000000000000000, -25.00000000000000000, 0.000000000000000000 ) ) ;
#11228 = ORIENTED_EDGE ( 'NONE', *, *, #3172, .T. ) ;
#11229 = CIRCLE ( 'NONE', #9313, 269.0000000000000000 ) ;
#11230 = CARTESIAN_POINT ( 'NONE',  ( 235.0999999999999943, 0.000000000000000000, 0.000000000000000000 ) ) ;
#11231 = CARTESIAN_POINT ( 'NONE',  ( 239.4141849554329724, 1.410389959096011392, 3.203344682971027702 ) ) ;
#11232 = DIRECTION ( 'NONE',  ( 0.000000000000000000, -1.000000000000000000, 0.000000000000000000 ) ) ;
#11233 = CARTESIAN_POINT ( 'NONE',  ( -197.8197553893909912, 30.00000000000000000, 64.27553482999130097 ) ) ;
#11234 = PRODUCT_DEFINITION_SHAPE ( 'NONE', 'NONE',  #13126 ) ;
#11235 = DIRECTION ( 'NONE',  ( 0.000000000000000000, 0.000000000000000000, 1.000000000000000000 ) ) ;
#11236 = AXIS2_PLACEMENT_3D ( 'NONE', #1225, #5285, #9361 ) ;
#11237 = FACE_OUTER_BOUND ( 'NONE', #3414, .T. ) ;
#11238 = ITEM_DEFINED_TRANSFORMATION ( 'NONE', 'NONE', #11236,  #805 ) ;
#11239 = VERTEX_POINT ( 'NONE', #2710 ) ;
#11240 = LINE ( 'NONE', #9450, #10715 ) ;
#11241 = ORIENTED_EDGE ( 'NONE', *, *, #9638, .F. ) ;
#11242 = DIRECTION ( 'NONE',  ( 0.000000000000000000, -0.01970892327970900221, -0.9998057603070482635 ) ) ;
#11243 = CARTESIAN_POINT ( 'NONE',  ( -243.4813404522815290, -7.728679802368493945, -9.179736092244947798 ) ) ;
#11244 = EDGE_CURVE ( 'NONE', #9162, #4030, #8730, .T. ) ;
#11245 = EDGE_CURVE ( 'NONE', #10853, #8685, #4438, .T. ) ;
#11246 = CARTESIAN_POINT ( 'NONE',  ( 6.345753394971347358E-13, 20.08915143297736350, -260.5542428351130866 ) ) ;
#11247 = CIRCLE ( 'NONE', #3581, 5.100000000000003197 ) ;
#11248 = ORIENTED_EDGE ( 'NONE', *, *, #10145, .T. ) ;
#11249 = CIRCLE ( 'NONE', #11037, 6.499999999999999112 ) ;
#11250 = VECTOR ( 'NONE', #3402, 1000.000000000000000 ) ;
#11251 = AXIS2_PLACEMENT_3D ( 'NONE', #9204, #12013, #2008 ) ;
#11252 = AXIS2_PLACEMENT_3D ( 'NONE', #5601, #3462, #2269 ) ;
#11253 = CARTESIAN_POINT ( 'NONE',  ( 234.3927740976959910, 20.79694577647348908, -115.5625104414818054 ) ) ;
#11254 = CARTESIAN_POINT ( 'NONE',  ( -245.5556485997058758, 9.020247694294253549, -7.914083889464029298 ) ) ;
#11255 = CARTESIAN_POINT ( 'NONE',  ( 185.9653539490014111, -30.00000000000000000, 225.1241593668316625 ) ) ;
#11256 = AXIS2_PLACEMENT_3D ( 'NONE', #6826, #1690, #10084 ) ;
#11257 = CARTESIAN_POINT ( 'NONE',  ( -243.6022064637596145, -7.815160977192930680, -8.774769252031678235 ) ) ;
#11258 = ADVANCED_FACE ( 'NONE', ( #7923 ), #11263, .F. ) ;
#11259 = DIRECTION ( 'NONE',  ( 0.000000000000000000, 1.000000000000000000, 0.000000000000000000 ) ) ;
#11260 = CARTESIAN_POINT ( 'NONE',  ( 41.85124196045095601, -138.4705547276867321, 4.383684909369697405E-13 ) ) ;
#11261 = CARTESIAN_POINT ( 'NONE',  ( -229.9651094064373638, 11.31238621391031529, -4.021116903567067524 ) ) ;
#11262 = CONTEXT_DEPENDENT_SHAPE_REPRESENTATION ( #12830, #10909 ) ;
#11263 = CONICAL_SURFACE ( 'NONE', #4224, 6.500000000000000888, 0.7853981633974617127 ) ;
#11264 = ADVANCED_BREP_SHAPE_REPRESENTATION ( '', ( #5911, #805 ), #1451 ) ;
#11265 = TOROIDAL_SURFACE ( 'NONE', #11901, 247.7999999999999829, 2.000000000000000000 ) ;
#11266 = DIRECTION ( 'NONE',  ( 0.000000000000000000, 1.000000000000000000, 0.000000000000000000 ) ) ;
#11267 = ORIENTED_EDGE ( 'NONE', *, *, #9962, .F. ) ;
#11268 = ORIENTED_EDGE ( 'NONE', *, *, #4351, .T. ) ;
#11269 = AXIS2_PLACEMENT_3D ( 'NONE', #7530, #4325, #12716 ) ;
#11270 = CARTESIAN_POINT ( 'NONE',  ( -260.5542428346390125, 20.08915143307225648, 17.05314194216809653 ) ) ;
#11271 = CARTESIAN_POINT ( 'NONE',  ( -197.8197553893909912, 30.00000000000000000, 64.27553482999130097 ) ) ;
#11272 = PRODUCT_DEFINITION_SHAPE ( 'NONE', 'NONE',  #13084 ) ;
#11273 = CARTESIAN_POINT ( 'NONE',  ( 239.1385365879861524, -0.8886010998478790501, -3.385772393335910291 ) ) ;
#11274 = AXIS2_PLACEMENT_3D ( 'NONE', #845, #6722, #1585 ) ;
#11275 = FACE_OUTER_BOUND ( 'NONE', #10782, .T. ) ;
#11276 = EDGE_CURVE ( 'NONE', #2870, #431, #1800, .T. ) ;
#11277 = CARTESIAN_POINT ( 'NONE',  ( 157.1762463448213225, -30.00000000000000000, 249.7084930171495500 ) ) ;
#11278 = ADVANCED_FACE ( 'NONE', ( #2908 ), #11473, .F. ) ;
#11279 = CARTESIAN_POINT ( 'NONE',  ( 0.000000000000000000, 0.000000000000000000, 0.000000000000000000 ) ) ;
#11280 = DIRECTION ( 'NONE',  ( 0.2588190451025314531, 0.000000000000000000, -0.9659258262890654256 ) ) ;
#11281 = CARTESIAN_POINT ( 'NONE',  ( -242.6830939053905638, -7.008887182000894889, 9.430537150680942560 ) ) ;
#11282 = ORIENTED_EDGE ( 'NONE', *, *, #2556, .F. ) ;
#11283 = CARTESIAN_POINT ( 'NONE',  ( 240.4181131690832558, -2.891045149246452617, -1.982248008101765935 ) ) ;
#11284 = AXIS2_PLACEMENT_3D ( 'NONE', #5370, #12500, #4422 ) ;
#11285 = LINE ( 'NONE', #9352, #3372 ) ;
#11286 = ORIENTED_EDGE ( 'NONE', *, *, #12761, .F. ) ;
#11287 = VERTEX_POINT ( 'NONE', #796 ) ;
#11288 = DIRECTION ( 'NONE',  ( 1.000000000000000000, 0.000000000000000000, 0.000000000000000000 ) ) ;
#11289 = DIRECTION ( 'NONE',  ( 0.000000000000000000, -1.000000000000000000, 0.000000000000000000 ) ) ;
#11290 = CARTESIAN_POINT ( 'NONE',  ( -17.09264059776470290, 19.96883746054087538, 261.1558126970361400 ) ) ;
#11291 = EDGE_CURVE ( 'NONE', #6697, #12416, #7225, .T. ) ;
#11292 = CARTESIAN_POINT ( 'NONE',  ( -239.1339513535814945, -1.403748199837580035, -11.91760216378363424 ) ) ;
#11293 = DIRECTION ( 'NONE',  ( -0.5735764363510471586, 0.000000000000000000, 0.8191520442889910214 ) ) ;
#11294 = CARTESIAN_POINT ( 'NONE',  ( -246.7375545285866849, 9.485935068452450381, 6.933947692770260574 ) ) ;
#11295 = AXIS2_PLACEMENT_3D ( 'NONE', #7863, #5668, #11865 ) ;
#11296 = ORIENTED_EDGE ( 'NONE', *, *, #2724, .F. ) ;
#11297 = CARTESIAN_POINT ( 'NONE',  ( -197.8197553893924976, 19.00000000000000000, -64.27553482998719403 ) ) ;
#11298 = EDGE_CURVE ( 'NONE', #552, #4800, #835, .T. ) ;
#11299 = VERTEX_POINT ( 'NONE', #6268 ) ;
#11300 = CIRCLE ( 'NONE', #7260, 246.0000000000000000 ) ;
#11301 = DIRECTION ( 'NONE',  ( -0.000000000000000000, -1.000000000000000000, 0.000000000000000000 ) ) ;
#11302 = EDGE_LOOP ( 'NONE', ( #3209, #8023 ) ) ;
#11303 = ORIENTED_EDGE ( 'NONE', *, *, #4594, .F. ) ;
#11304 =( REPRESENTATION_RELATIONSHIP ('NONE','NONE', #12019, #5191 ) REPRESENTATION_RELATIONSHIP_WITH_TRANSFORMATION ( #8668 )SHAPE_REPRESENTATION_RELATIONSHIP( ) );
#11305 = CARTESIAN_POINT ( 'NONE',  ( -197.8197553893909912, 19.00000000000000000, 69.77553482999131518 ) ) ;
#11306 = CARTESIAN_POINT ( 'NONE',  ( 67.76049180374880621, 20.55460285150727273, 252.9796497720274147 ) ) ;
#11307 =( NAMED_UNIT ( * ) SI_UNIT ( $, .STERADIAN. ) SOLID_ANGLE_UNIT ( ) );
#11308 = CARTESIAN_POINT ( 'NONE',  ( -27.68945685411286561, -30.00000000000000000, 290.6841825403027997 ) ) ;
#11309 = FACE_OUTER_BOUND ( 'NONE', #11226, .T. ) ;
#11310 = CARTESIAN_POINT ( 'NONE',  ( 138.9238112054132159, -25.00000000000000000, -212.6409525001303962 ) ) ;
#11311 = CARTESIAN_POINT ( 'NONE',  ( -185.9653539489998195, -29.00000000000000000, -225.1241593668329699 ) ) ;
#11312 = CONTEXT_DEPENDENT_SHAPE_REPRESENTATION ( #3864, #9876 ) ;
#11313 = ORIENTED_EDGE ( 'NONE', *, *, #6903, .T. ) ;
#11314 = CARTESIAN_POINT ( 'NONE',  ( 0.000000000000000000, -9.997999799959989886, 0.000000000000000000 ) ) ;
#11315 = CIRCLE ( 'NONE', #7479, 240.3921568627444856 ) ;
#11316 = AXIS2_PLACEMENT_3D ( 'NONE', #668, #3976, #5857 ) ;
#11317 = ORIENTED_EDGE ( 'NONE', *, *, #6868, .F. ) ;
#11318 = LINE ( 'NONE', #1190, #190 ) ;
#11319 = CARTESIAN_POINT ( 'NONE',  ( -246.2429388857162280, -9.313684383457655258, -7.566737218363915218 ) ) ;
#11320 = CARTESIAN_POINT ( 'NONE',  ( -248.8244828231703138, -10.12360735459863115, 5.964490512234371877 ) ) ;
#11321 = ORIENTED_EDGE ( 'NONE', *, *, #9993, .F. ) ;
#11322 = CARTESIAN_POINT ( 'NONE',  ( 67.61424743078299571, 20.79694577590440119, 252.4341100442090067 ) ) ;
#11323 = CARTESIAN_POINT ( 'NONE',  ( -245.0420335974988006, 8.761757997507153561, -8.199751242572485666 ) ) ;
#11324 = DIRECTION ( 'NONE',  ( 0.6368676505102696117, 0.000000000000000000, 0.7709731485165545184 ) ) ;
#11325 = CARTESIAN_POINT ( 'NONE',  ( -245.4374131367196696, -8.957880036294859849, -7.603877363506748921 ) ) ;
#11326 =( REPRESENTATION_RELATIONSHIP ('NONE','NONE', #12019, #5191 ) REPRESENTATION_RELATIONSHIP_WITH_TRANSFORMATION ( #1454 )SHAPE_REPRESENTATION_RELATIONSHIP( ) );
#11327 = VECTOR ( 'NONE', #6677, 1000.000000000000000 ) ;
#11328 = EDGE_CURVE ( 'NONE', #3016, #5226, #615, .T. ) ;
#11329 = CARTESIAN_POINT ( 'NONE',  ( 239.2050160255199955, -1.043887935101727393, 3.340720568042238714 ) ) ;
#11330 = DIRECTION ( 'NONE',  ( 0.5735764363510555963, 0.000000000000000000, -0.8191520442889851372 ) ) ;
#11331 = CARTESIAN_POINT ( 'NONE',  ( 240.6324715326043702, 3.499918298005177952, 0.3875926901506949740 ) ) ;
#11332 = CIRCLE ( 'NONE', #13030, 5.500000000000007994 ) ;
#11333 = DIRECTION ( 'NONE',  ( 1.000000000000000000, 0.000000000000000000, 0.000000000000000000 ) ) ;
#11334 = ORIENTED_EDGE ( 'NONE', *, *, #3606, .F. ) ;
#11335 = AXIS2_PLACEMENT_3D ( 'NONE', #10418, #11425, #1293 ) ;
#11336 = CARTESIAN_POINT ( 'NONE',  ( 67.55708173931988370, 20.08915143256180968, 252.2208631684339935 ) ) ;
#11337 = LINE ( 'NONE', #342, #8284 ) ;
#11338 = AXIS2_PLACEMENT_3D ( 'NONE', #7247, #5166, #8116 ) ;
#11339 = CARTESIAN_POINT ( 'NONE',  ( -122.2593324768321992, 30.00000000000000000, 168.2755348299905052 ) ) ;
#11340 = LINE ( 'NONE', #3125, #11809 ) ;
#11341 = CARTESIAN_POINT ( 'NONE',  ( -248.6652334677784779, -9.923450225169199612, 6.747319395809158848 ) ) ;
#11342 = EDGE_CURVE ( 'NONE', #8497, #12659, #4854, .T. ) ;
#11343 = CARTESIAN_POINT ( 'NONE',  ( -293.0608542803120145, -19.40000000000000213, 6.485521991431949296 ) ) ;
#11344 = DIRECTION ( 'NONE',  ( 0.7071067811865561215, 0.000000000000000000, -0.7071067811865389130 ) ) ;
#11345 = AXIS2_PLACEMENT_3D ( 'NONE', #10400, #8286, #9410 ) ;
#11346 = DIRECTION ( 'NONE',  ( 0.000000000000000000, 0.000000000000000000, 1.000000000000000000 ) ) ;
#11347 = ORIENTED_EDGE ( 'NONE', *, *, #6407, .F. ) ;
#11348 = VECTOR ( 'NONE', #8897, 1000.000000000000000 ) ;
#11349 = DIRECTION ( 'NONE',  ( -0.6368676505102707219, 0.000000000000000000, -0.7709731485165535192 ) ) ;
#11350 = CARTESIAN_POINT ( 'NONE',  ( 229.9973412510026662, -3.321846415627111693, -1.126016662849602223 ) ) ;
#11351 = EDGE_LOOP ( 'NONE', ( #11241, #7670, #1352, #11415 ) ) ;
#11352 = EDGE_LOOP ( 'NONE', ( #8461, #5223, #172, #1150, #4764 ) ) ;
#11353 = EDGE_CURVE ( 'NONE', #4274, #10097, #7426, .T. ) ;
#11354 = EDGE_CURVE ( 'NONE', #13033, #982, #24, .T. ) ;
#11355 = DIRECTION ( 'NONE',  ( 0.6368676505102707219, 0.000000000000000000, 0.7709731485165535192 ) ) ;
#11356 = CARTESIAN_POINT ( 'NONE',  ( 0.000000000000000000, 29.00000000000000000, 208.0000000000000000 ) ) ;
#11357 = VECTOR ( 'NONE', #8477, 1000.000000000000000 ) ;
#11358 = CIRCLE ( 'NONE', #6254, 195.0000000000000000 ) ;
#11359 = AXIS2_PLACEMENT_3D ( 'NONE', #5485, #301, #12618 ) ;
#11360 = CARTESIAN_POINT ( 'NONE',  ( -172.6991790963936921, 20.55460285138878618, 196.8887528212225106 ) ) ;
#11361 = CARTESIAN_POINT ( 'NONE',  ( 0.000000000000000000, -3.327561323230890267, 0.000000000000000000 ) ) ;
#11362 = CIRCLE ( 'NONE', #12632, 304.0000000000000000 ) ;
#11363 = CARTESIAN_POINT ( 'NONE',  ( 0.000000000000000000, 0.000000000000000000, 0.000000000000000000 ) ) ;
#11364 = CARTESIAN_POINT ( 'NONE',  ( -243.3200464879880371, 7.587187391486287069, 8.972284947528141430 ) ) ;
#11365 = VERTEX_POINT ( 'NONE', #195 ) ;
#11366 = DIRECTION ( 'NONE',  ( 1.000000000000000000, 0.000000000000000000, 0.000000000000000000 ) ) ;
#11367 = CIRCLE ( 'NONE', #12645, 0.8000000000000003775 ) ;
#11368 = ORIENTED_EDGE ( 'NONE', *, *, #13038, .F. ) ;
#11369 = FACE_OUTER_BOUND ( 'NONE', #5291, .T. ) ;
#11370 = ORIENTED_EDGE ( 'NONE', *, *, #10395, .T. ) ;
#11371 = ORIENTED_EDGE ( 'NONE', *, *, #3862, .T. ) ;
#11372 = EDGE_CURVE ( 'NONE', #3155, #1462, #8066, .T. ) ;
#11373 = EDGE_CURVE ( 'NONE', #3138, #9134, #12533, .T. ) ;
#11374 =( REPRESENTATION_RELATIONSHIP ('NONE','NONE', #12019, #182 ) REPRESENTATION_RELATIONSHIP_WITH_TRANSFORMATION ( #11444 )SHAPE_REPRESENTATION_RELATIONSHIP( ) );
#11375 = DIRECTION ( 'NONE',  ( -0.000000000000000000, -1.000000000000000000, 0.000000000000000000 ) ) ;
#11376 = CARTESIAN_POINT ( 'NONE',  ( 235.4000000000000057, -4.447920636657316074, 2.686261716586446635 ) ) ;
#11377 = DIRECTION ( 'NONE',  ( 8.659560562354913137E-17, -0.7071067811865489050, 0.7071067811865460184 ) ) ;
#11378 = VECTOR ( 'NONE', #7115, 1000.000000000000000 ) ;
#11379 = ADVANCED_FACE ( 'NONE', ( #6066 ), #8332, .F. ) ;
#11380 = CARTESIAN_POINT ( 'NONE',  ( 2.394184492333075617E-14, 29.00000000000000000, -195.0000000000000000 ) ) ;
#11381 = CARTESIAN_POINT ( 'NONE',  ( -294.8238222686198355, -30.00000000000000000, -32.70078231947154279 ) ) ;
#11382 = ITEM_DEFINED_TRANSFORMATION ( 'NONE', 'NONE', #6786,  #805 ) ;
#11383 = ORIENTED_EDGE ( 'NONE', *, *, #6529, .T. ) ;
#11384 = CYLINDRICAL_SURFACE ( 'NONE', #11142, 5.500000000000015099 ) ;
#11385 = ORIENTED_EDGE ( 'NONE', *, *, #11937, .F. ) ;
#11386 = CARTESIAN_POINT ( 'NONE',  ( -4.572608844893758122E-13, 20.79694577634647601, 260.7745447061711275 ) ) ;
#11387 = CARTESIAN_POINT ( 'NONE',  ( -247.0236966365115450, -9.579141830393634649, -7.227478268642161474 ) ) ;
#11388 = PRODUCT_DEFINITION_SHAPE ( 'NONE', 'NONE',  #13088 ) ;
#11389 = CIRCLE ( 'NONE', #6501, 2.000000000000000444 ) ;
#11390 = EDGE_CURVE ( 'NONE', #8118, #2005, #1994, .T. ) ;
#11391 = CARTESIAN_POINT ( 'NONE',  ( 240.3826708216964789, -2.772967769359314882, -2.135567781667015108 ) ) ;
#11392 = ORIENTED_EDGE ( 'NONE', *, *, #5154, .T. ) ;
#11393 = CARTESIAN_POINT ( 'NONE',  ( 159.0697709852749995, 20.79694577591498472, -207.3438552938715134 ) ) ;
#11394 = CARTESIAN_POINT ( 'NONE',  ( -240.5255509705628469, 3.902938849068647631, -11.34756747382315112 ) ) ;
#11395 = CARTESIAN_POINT ( 'NONE',  ( 140.0242476638101152, -18.00000000000000000, -251.1826895432237166 ) ) ;
#11396 = CARTESIAN_POINT ( 'NONE',  ( -244.0507507057079977, -8.147415050172172712, -8.468315434781628070 ) ) ;
#11397 = CIRCLE ( 'NONE', #12882, 248.1666666666679930 ) ;
#11398 = FILL_AREA_STYLE ('',( #261 ) ) ;
#11399 = PRODUCT_DEFINITION_SHAPE ( 'NONE', 'NONE',  #6540 ) ;
#11400 = APPLICATION_PROTOCOL_DEFINITION ( 'draft international standard', 'automotive_design', 1998, #13001 ) ;
#11401 = DIRECTION ( 'NONE',  ( 0.6368676505102707219, 0.000000000000000000, 0.7709731485165535192 ) ) ;
#11402 = DIRECTION ( 'NONE',  ( 0.000000000000000000, 0.01970892327970883220, 0.9998057603070481525 ) ) ;
#11403 = EDGE_LOOP ( 'NONE', ( #12223, #7140 ) ) ;
#11404 = CIRCLE ( 'NONE', #6519, 5.500000000000015099 ) ;
#11405 = CARTESIAN_POINT ( 'NONE',  ( 207.1687172302655142, 20.08915143321463503, -158.9353507248590063 ) ) ;
#11406 = FACE_OUTER_BOUND ( 'NONE', #3223, .T. ) ;
#11407 = CONICAL_SURFACE ( 'NONE', #5653, 1.750000000000000000, 0.4188790204786330129 ) ;
#11408 = DIRECTION ( 'NONE',  ( -0.7709731485165536302, 0.000000000000000000, 0.6368676505102706109 ) ) ;
#11409 = CARTESIAN_POINT ( 'NONE',  ( 6.735557395310435121E-16, 19.00000000000000000, -213.5000000000000000 ) ) ;
#11410 = DIRECTION ( 'NONE',  ( 1.000000000000000000, 0.000000000000000000, 1.421085471520200056E-14 ) ) ;
#11411 = CARTESIAN_POINT ( 'NONE',  ( -248.3022220597990781, -9.870789006701004453, 6.824104388389867104 ) ) ;
#11412 = FACE_OUTER_BOUND ( 'NONE', #6946, .T. ) ;
#11413 = DIRECTION ( 'NONE',  ( 0.9063077870366453848, 0.000000000000000000, 0.4226182617407092668 ) ) ;
#11414 = CARTESIAN_POINT ( 'NONE',  ( -0.000000000000000000, -25.00000000000000000, 0.000000000000000000 ) ) ;
#11415 = ORIENTED_EDGE ( 'NONE', *, *, #10168, .T. ) ;
#11416 = CARTESIAN_POINT ( 'NONE',  ( 122.2593324768346008, 30.00000000000000000, 162.7755348299889988 ) ) ;
#11417 = CARTESIAN_POINT ( 'NONE',  ( 229.9785086005968537, -1.552204380456203348, 3.145362046007984080 ) ) ;
#11418 = VERTEX_POINT ( 'NONE', #69 ) ;
#11419 = EDGE_CURVE ( 'NONE', #6421, #2427, #1890, .T. ) ;
#11420 = ORIENTED_EDGE ( 'NONE', *, *, #6606, .T. ) ;
#11421 = EDGE_CURVE ( 'NONE', #12564, #4415, #8265, .T. ) ;
#11422 = DIRECTION ( 'NONE',  ( 0.6368676505102707219, 0.000000000000000000, 0.7709731485165535192 ) ) ;
#11423 = DIRECTION ( 'NONE',  ( 0.000000000000000000, -1.000000000000000000, 0.000000000000000000 ) ) ;
#11424 = CARTESIAN_POINT ( 'NONE',  ( -261.3381329044966606, 20.55460285096646089, -17.10461161606123426 ) ) ;
#11425 = DIRECTION ( 'NONE',  ( 0.000000000000000000, 1.000000000000000000, 0.000000000000000000 ) ) ;
#11426 = CARTESIAN_POINT ( 'NONE',  ( 0.000000000000000000, 0.000000000000000000, 0.000000000000000000 ) ) ;
#11427 = DIRECTION ( 'NONE',  ( -0.000000000000000000, 1.000000000000000000, 0.000000000000000000 ) ) ;
#11428 = ADVANCED_FACE ( 'NONE', ( #3047 ), #992, .F. ) ;
#11429 = ORIENTED_EDGE ( 'NONE', *, *, #1507, .F. ) ;
#11430 = DIRECTION ( 'NONE',  ( -1.000000000000000000, 0.000000000000000000, 0.000000000000000000 ) ) ;
#11431 = ORIENTED_EDGE ( 'NONE', *, *, #3204, .F. ) ;
#11432 = CARTESIAN_POINT ( 'NONE',  ( -0.000000000000000000, -25.50000000000000000, 0.000000000000000000 ) ) ;
#11433 = VERTEX_POINT ( 'NONE', #4252 ) ;
#11434 = ORIENTED_EDGE ( 'NONE', *, *, #3719, .T. ) ;
#11435 = DIRECTION ( 'NONE',  ( 0.000000000000000000, 1.000000000000000000, 0.000000000000000000 ) ) ;
#11436 = SURFACE_SIDE_STYLE ('',( #9240 ) ) ;
#11437 = LINE ( 'NONE', #2238, #5304 ) ;
#11438 = CARTESIAN_POINT ( 'NONE',  ( 0.000000000000000000, 19.00000000000000000, 202.4999999999999716 ) ) ;
#11439 = CARTESIAN_POINT ( 'NONE',  ( -238.7146392957941430, 0.1450841617578550458, -11.74918863377693690 ) ) ;
#11440 = CARTESIAN_POINT ( 'NONE',  ( -247.6855308008555596, 9.751870871517551720, 6.992977237921749634 ) ) ;
#11441 =( NAMED_UNIT ( * ) SI_UNIT ( $, .STERADIAN. ) SOLID_ANGLE_UNIT ( ) );
#11442 = ADVANCED_FACE ( 'NONE', ( #9121 ), #7062, .T. ) ;
#11443 = EDGE_CURVE ( 'NONE', #11485, #1281, #10179, .T. ) ;
#11444 = ITEM_DEFINED_TRANSFORMATION ( 'NONE', 'NONE', #12097,  #805 ) ;
#11445 = ORIENTED_EDGE ( 'NONE', *, *, #8588, .F. ) ;
#11446 = DIRECTION ( 'NONE',  ( 1.000000000000000000, 0.000000000000000000, 0.000000000000000000 ) ) ;
#11448 = VERTEX_POINT ( 'NONE', #1928 ) ;
#11447 = AXIS2_PLACEMENT_3D ( 'NONE', #6591, #6397, #6463 ) ;
#11449 =( REPRESENTATION_RELATIONSHIP ('NONE','NONE', #12019, #182 ) REPRESENTATION_RELATIONSHIP_WITH_TRANSFORMATION ( #9505 )SHAPE_REPRESENTATION_RELATIONSHIP( ) );
#11450 = DIRECTION ( 'NONE',  ( -0.6368676505102707219, 0.000000000000000000, -0.7709731485165535192 ) ) ;
#11451 = DIRECTION ( 'NONE',  ( -0.000000000000000000, -1.000000000000000000, 0.000000000000000000 ) ) ;
#11452 = DIRECTION ( 'NONE',  ( 0.000000000000000000, 1.000000000000000000, 0.000000000000000000 ) ) ;
#11453 = ORIENTED_EDGE ( 'NONE', *, *, #4996, .F. ) ;
#11454 = DIRECTION ( 'NONE',  ( 1.000000000000000000, 0.000000000000000000, 0.000000000000000000 ) ) ;
#11455 = CARTESIAN_POINT ( 'NONE',  ( -244.0248830888228895, 8.135989420001589423, -8.821260460353125055 ) ) ;
#11456 = FACE_OUTER_BOUND ( 'NONE', #9984, .T. ) ;
#11457 = CARTESIAN_POINT ( 'NONE',  ( -197.8197553893924976, 30.00000000000000000, -70.77553482998720824 ) ) ;
#11458 = AXIS2_PLACEMENT_3D ( 'NONE', #11426, #5220, #2028 ) ;
#11459 = EDGE_CURVE ( 'NONE', #11287, #5843, #7001, .T. ) ;
#11460 = DIRECTION ( 'NONE',  ( 0.9961946980917466554, 0.000000000000000000, -0.08715574274764503748 ) ) ;
#11461 = DIRECTION ( 'NONE',  ( 0.000000000000000000, 0.9998057603070480415, -0.01970892327970899874 ) ) ;
#11462 = CONTEXT_DEPENDENT_SHAPE_REPRESENTATION ( #8852, #6757 ) ;
#11463 = AXIS2_PLACEMENT_3D ( 'NONE', #425, #10616, #2355 ) ;
#11464 = CARTESIAN_POINT ( 'NONE',  ( -210.0000000000000000, 30.00000000000000000, 0.000000000000000000 ) ) ;
#11465 = EDGE_LOOP ( 'NONE', ( #3894, #2685, #12189, #10939 ) ) ;
#11466 = CARTESIAN_POINT ( 'NONE',  ( -159.3024069656823940, 19.96883745967399548, 207.6469600131863729 ) ) ;
#11467 = CARTESIAN_POINT ( 'NONE',  ( -189.4681260268063170, -30.00000000000000000, -229.3645116836740385 ) ) ;
#11468 = LINE ( 'NONE', #2397, #3806 ) ;
#11469 = CARTESIAN_POINT ( 'NONE',  ( 197.8197553893920144, 30.00000000000000000, 64.27553482998850143 ) ) ;
#11470 = CARTESIAN_POINT ( 'NONE',  ( 227.3999999999999773, 0.1024105694487990881, 5.195143123655512341 ) ) ;
#11471 = AXIS2_PLACEMENT_3D ( 'NONE', #3567, #11783, #12643 ) ;
#11472 =( REPRESENTATION_RELATIONSHIP ('NONE','NONE', #12019, #5191 ) REPRESENTATION_RELATIONSHIP_WITH_TRANSFORMATION ( #9129 )SHAPE_REPRESENTATION_RELATIONSHIP( ) );
#11473 = CONICAL_SURFACE ( 'NONE', #10188, 250.1999999999999602, 0.7853981633974758125 ) ;
#11474 = CYLINDRICAL_SURFACE ( 'NONE', #11522, 249.7999999999999829 ) ;
#11475 = DIRECTION ( 'NONE',  ( -0.8294267566935212832, 0.5538822189107471816, 0.07256543843575528896 ) ) ;
#11476 = CIRCLE ( 'NONE', #8067, 5.500000000000005329 ) ;
#11477 = DIRECTION ( 'NONE',  ( 0.6368676505102709440, 0.000000000000000000, 0.7709731485165532971 ) ) ;
#11478 = AXIS2_PLACEMENT_3D ( 'NONE', #2941, #7090, #1019 ) ;
#11479 = ITEM_DEFINED_TRANSFORMATION ( 'NONE', 'NONE', #2093,  #805 ) ;
#11480 = ORIENTED_EDGE ( 'NONE', *, *, #5156, .T. ) ;
#11481 = AXIS2_PLACEMENT_3D ( 'NONE', #4517, #10855, #4646 ) ;
#11482 = CARTESIAN_POINT ( 'NONE',  ( 240.5163796274145511, -3.187645493303870037, 1.494965077496835049 ) ) ;
#11483 = CONICAL_SURFACE ( 'NONE', #6161, 6.500000000000005329, 0.7853981633974476129 ) ;
#11484 = CARTESIAN_POINT ( 'NONE',  ( -229.9035141788515375, -9.983227244538054990, 6.668950963032000523 ) ) ;
#11485 = VERTEX_POINT ( 'NONE', #9192 ) ;
#11486 = ORIENTED_EDGE ( 'NONE', *, *, #3438, .T. ) ;
#11487 = CIRCLE ( 'NONE', #6168, 6.500000000000000888 ) ;
#11488 = CARTESIAN_POINT ( 'NONE',  ( -122.2593324768359935, 29.00000000000000000, -168.2755348299880040 ) ) ;
#11489 = DIRECTION ( 'NONE',  ( 0.000000000000000000, -1.000000000000000000, 0.000000000000000000 ) ) ;
#11490 = CARTESIAN_POINT ( 'NONE',  ( -84.20717312374198116, 20.55460285077014504, 247.9906035358103225 ) ) ;
#11491 = DIRECTION ( 'NONE',  ( 0.000000000000000000, -0.8560027256360642767, 0.5169713083949908361 ) ) ;
#11492 = DIRECTION ( 'NONE',  ( -0.5000000000000041078, 0.000000000000000000, 0.8660254037844364872 ) ) ;
#11493 = DIRECTION ( 'NONE',  ( 1.000000000000000000, 0.000000000000000000, 0.000000000000000000 ) ) ;
#11494 = ADVANCED_FACE ( 'NONE', ( #4122 ), #2531, .T. ) ;
#11495 = FACE_OUTER_BOUND ( 'NONE', #6239, .T. ) ;
#11496 = EDGE_CURVE ( 'NONE', #5907, #3553, #4012, .T. ) ;
#11497 = AXIS2_PLACEMENT_3D ( 'NONE', #4553, #4477, #11771 ) ;
#11498 = ORIENTED_EDGE ( 'NONE', *, *, #4895, .F. ) ;
#11499 = DIRECTION ( 'NONE',  ( 0.000000000000000000, 0.000000000000000000, 1.000000000000000000 ) ) ;
#11500 = AXIS2_PLACEMENT_3D ( 'NONE', #12646, #1387, #3437 ) ;
#11501 = EDGE_LOOP ( 'NONE', ( #11886, #11210 ) ) ;
#11502 = CARTESIAN_POINT ( 'NONE',  ( -197.8197553893924976, 30.00000000000000000, -58.77553482998720114 ) ) ;
#11503 = ORIENTED_EDGE ( 'NONE', *, *, #11390, .T. ) ;
#11504 = ORIENTED_EDGE ( 'NONE', *, *, #3938, .T. ) ;
#11505 = CIRCLE ( 'NONE', #2971, 6.500000000000005329 ) ;
#11506 = DIRECTION ( 'NONE',  ( 0.000000000000000000, 1.000000000000000000, 0.000000000000000000 ) ) ;
#11507 = PRODUCT_DEFINITION_SHAPE ( 'NONE', 'NONE',  #13048 ) ;
#11508 = CYLINDRICAL_SURFACE ( 'NONE', #2541, 1.750000000000000000 ) ;
#11509 = DIRECTION ( 'NONE',  ( -0.6368676505102707219, 0.000000000000000000, -0.7709731485165536302 ) ) ;
#11510 = AXIS2_PLACEMENT_3D ( 'NONE', #4655, #3929, #9928 ) ;
#11511 = CARTESIAN_POINT ( 'NONE',  ( -238.8528788548577779, 0.8456725619206635347, -11.72072902431185959 ) ) ;
#11512 = CARTESIAN_POINT ( 'NONE',  ( -249.7118339206215012, 9.997999799959989886, -6.636264009214830395 ) ) ;
#11513 = FILL_AREA_STYLE_COLOUR ( '', #8156 ) ;
#11514 = EDGE_CURVE ( 'NONE', #2818, #6490, #2187, .T. ) ;
#11515 = CONTEXT_DEPENDENT_SHAPE_REPRESENTATION ( #9145, #10826 ) ;
#11516 = VECTOR ( 'NONE', #8481, 1000.000000000000000 ) ;
#11517 = EDGE_LOOP ( 'NONE', ( #1873, #8294, #1315 ) ) ;
#11518 = CYLINDRICAL_SURFACE ( 'NONE', #10933, 249.7999999999999829 ) ;
#11519 = EDGE_LOOP ( 'NONE', ( #8161, #920, #592, #5275 ) ) ;
#11520 = CARTESIAN_POINT ( 'NONE',  ( 0.000000000000000000, 30.00000000000000000, 196.0000000000000000 ) ) ;
#11521 = FACE_OUTER_BOUND ( 'NONE', #10851, .T. ) ;
#11522 = AXIS2_PLACEMENT_3D ( 'NONE', #11279, #5204, #9279 ) ;
#11523 = CARTESIAN_POINT ( 'NONE',  ( 158.7026972336036579, 20.08915143297736705, -206.8203823583188807 ) ) ;
#11524 = ORIENTED_EDGE ( 'NONE', *, *, #5734, .F. ) ;
#11525 = EDGE_CURVE ( 'NONE', #10752, #5691, #9343, .T. ) ;
#11526 = CARTESIAN_POINT ( 'NONE',  ( 235.4000000000000057, 2.999417280921144346, -0.05912676983912663192 ) ) ;
#11527 = ADVANCED_FACE ( 'NONE', ( #5516 ), #5524, .F. ) ;
#11528 = CARTESIAN_POINT ( 'NONE',  ( -240.9947549591053928, 4.840187564906756279, -10.98379185745642239 ) ) ;
#11529 = CARTESIAN_POINT ( 'NONE',  ( -225.1241593668336236, -30.00000000000000000, 185.9653539489990521 ) ) ;
#11530 = CARTESIAN_POINT ( 'NONE',  ( -240.6798348123905669, -4.210664053393288420, -10.96963869240667755 ) ) ;
#11531 = ORIENTED_EDGE ( 'NONE', *, *, #10342, .T. ) ;
#11532 = CARTESIAN_POINT ( 'NONE',  ( 239.4717458110699226, -1.490203034777392022, 3.166904956833142215 ) ) ;
#11533 = TOROIDAL_SURFACE ( 'NONE', #9572, 250.3823410207189966, 3.000000000000000000 ) ;
#11534 = CARTESIAN_POINT ( 'NONE',  ( 240.3826708216974737, 2.772967769358989809, 2.135567781667440102 ) ) ;
#11535 = ITEM_DEFINED_TRANSFORMATION ( 'NONE', 'NONE', #4676,  #805 ) ;
#11536 = VECTOR ( 'NONE', #7705, 1000.000000000000000 ) ;
#11537 = CARTESIAN_POINT ( 'NONE',  ( 7.960204194457791533E-16, 18.00000000000000000, 214.5000000000000000 ) ) ;
#11538 = ORIENTED_EDGE ( 'NONE', *, *, #10125, .T. ) ;
#11539 = CARTESIAN_POINT ( 'NONE',  ( -249.7931653183007086, -11.67801679920997593, -1.333825740846608321 ) ) ;
#11540 = CARTESIAN_POINT ( 'NONE',  ( 17.09264059776268851, 19.96883746064459331, 261.1558126970361400 ) ) ;
#11541 = ADVANCED_FACE ( 'NONE', ( #11456 ), #9576, .F. ) ;
#11542 = CARTESIAN_POINT ( 'NONE',  ( 159.2169126275676945, -3.061616997868385015E-14, 192.7432871291383663 ) ) ;
#11543 = FACE_OUTER_BOUND ( 'NONE', #10686, .T. ) ;
#11544 = CARTESIAN_POINT ( 'NONE',  ( 0.000000000000000000, 0.000000000000000000, 0.000000000000000000 ) ) ;
#11545 = DIRECTION ( 'NONE',  ( 0.000000000000000000, 0.000000000000000000, 1.000000000000000000 ) ) ;
#11546 = EDGE_CURVE ( 'NONE', #4563, #982, #2735, .T. ) ;
#11547 = DIRECTION ( 'NONE',  ( 0.000000000000000000, 0.000000000000000000, -1.000000000000000000 ) ) ;
#11548 = CARTESIAN_POINT ( 'NONE',  ( -17.68709912901524106, -138.4705547276867321, 37.93010648591168632 ) ) ;
#11549 = DIRECTION ( 'NONE',  ( 0.000000000000000000, -1.000000000000000000, 0.000000000000000000 ) ) ;
#11550 = ITEM_DEFINED_TRANSFORMATION ( 'NONE', 'NONE', #1071,  #805 ) ;
#11551 = VECTOR ( 'NONE', #3160, 1000.000000000000000 ) ;
#11552 = DIRECTION ( 'NONE',  ( 0.000000000000000000, 0.000000000000000000, 1.000000000000000000 ) ) ;
#11553 = VECTOR ( 'NONE', #3494, 1000.000000000000000 ) ;
#11554 = ORIENTED_EDGE ( 'NONE', *, *, #3376, .T. ) ;
#11555 = VERTEX_POINT ( 'NONE', #11395 ) ;
#11556 = FACE_OUTER_BOUND ( 'NONE', #8674, .T. ) ;
#11557 = FACE_BOUND ( 'NONE', #3817, .T. ) ;
#11558 = AXIS2_PLACEMENT_3D ( 'NONE', #3736, #940, #10998 ) ;
#11559 = CARTESIAN_POINT ( 'NONE',  ( 130.8783844628973441, 19.96883745980737501, -226.6392846544037809 ) ) ;
#11560 = DIRECTION ( 'NONE',  ( 0.6368676505102708330, 0.000000000000000000, 0.7709731485165535192 ) ) ;
#11561 = DIRECTION ( 'NONE',  ( 0.4226182617406972208, 0.000000000000000000, 0.9063077870366510469 ) ) ;
#11562 = AXIS2_PLACEMENT_3D ( 'NONE', #12897, #8967, #12829 ) ;
#11563 = FACE_OUTER_BOUND ( 'NONE', #3846, .T. ) ;
#11564 = CARTESIAN_POINT ( 'NONE',  ( -254.0989678903619051, 20.79694577634646535, 59.24444182677424919 ) ) ;
#11565 = ORIENTED_EDGE ( 'NONE', *, *, #10145, .F. ) ;
#11566 = CARTESIAN_POINT ( 'NONE',  ( 225.9597979674045405, 20.79694577634646535, -130.4544329367267324 ) ) ;
#11567 = EDGE_LOOP ( 'NONE', ( #8921, #8923, #7251, #11248 ) ) ;
#11568 = DIRECTION ( 'NONE',  ( 0.000000000000000000, 1.000000000000000000, 0.000000000000000000 ) ) ;
#11569 = ORIENTED_EDGE ( 'NONE', *, *, #1074, .T. ) ;
#11570 = ORIENTED_EDGE ( 'NONE', *, *, #2205, .T. ) ;
#11571 = VECTOR ( 'NONE', #3742, 1000.000000000000114 ) ;
#11572 = EDGE_CURVE ( 'NONE', #6137, #5558, #5187, .T. ) ;
#11573 = CARTESIAN_POINT ( 'NONE',  ( 287.1814104624967854, -30.00000000000000000, 23.44910453727082356 ) ) ;
#11574 = DIRECTION ( 'NONE',  ( -0.000000000000000000, -1.000000000000000000, 0.000000000000000000 ) ) ;
#11575 = CARTESIAN_POINT ( 'NONE',  ( -197.8197553893924976, 19.00000000000000000, -64.27553482998719403 ) ) ;
#11576 = CARTESIAN_POINT ( 'NONE',  ( -239.3871000706272696, 1.704623200064774302, -11.62580518457323642 ) ) ;
#11577 =( NAMED_UNIT ( * ) SI_UNIT ( $, .STERADIAN. ) SOLID_ANGLE_UNIT ( ) );
#11578 = DIRECTION ( 'NONE',  ( -0.000000000000000000, -1.000000000000000000, 0.000000000000000000 ) ) ;
#11579 = CIRCLE ( 'NONE', #6253, 195.0000000000000000 ) ;
#11580 = AXIS2_PLACEMENT_3D ( 'NONE', #7769, #8580, #11583 ) ;
#11581 = CONTEXT_DEPENDENT_SHAPE_REPRESENTATION ( #10512, #11272 ) ;
#11582 = VERTEX_POINT ( 'NONE', #4383 ) ;
#11583 = DIRECTION ( 'NONE',  ( 0.000000000000000000, 0.9998057603070481525, -0.01970892327970900221 ) ) ;
#11584 = EDGE_LOOP ( 'NONE', ( #123, #3332 ) ) ;
#11585 =( REPRESENTATION_RELATIONSHIP ('NONE','NONE', #12019, #5191 ) REPRESENTATION_RELATIONSHIP_WITH_TRANSFORMATION ( #395 )SHAPE_REPRESENTATION_RELATIONSHIP( ) );
#11586 = CARTESIAN_POINT ( 'NONE',  ( -241.3198063618330877, 5.342363202599722527, -10.46527477498853820 ) ) ;
#11587 = CARTESIAN_POINT ( 'NONE',  ( 135.8846079354933352, -19.40000000000000213, -256.1940150085812888 ) ) ;
#11588 = EDGE_CURVE ( 'NONE', #1904, #4880, #9559, .T. ) ;
#11589 = EDGE_CURVE ( 'NONE', #941, #10853, #4441, .T. ) ;
#11590 = AXIS2_PLACEMENT_3D ( 'NONE', #12558, #11698, #5431 ) ;
#11591 = FACE_OUTER_BOUND ( 'NONE', #5811, .T. ) ;
#11592 = CARTESIAN_POINT ( 'NONE',  ( -244.1671264060107660, 8.232476465879829064, -8.730683390178871406 ) ) ;
#11593 = CARTESIAN_POINT ( 'NONE',  ( -238.7604407559926187, 0.5508784862251008274, 11.98739478578908013 ) ) ;
#11594 = VECTOR ( 'NONE', #12340, 1000.000000000000114 ) ;
#11595 = CARTESIAN_POINT ( 'NONE',  ( -229.7148150354796314, 2.664985348179264690, 11.45030177774321167 ) ) ;
#11596 = SHAPE_REPRESENTATION ( 'External Heavy Duty Rotating Flange Ring', ( #805 ), #7613 ) ;
#11597 = CARTESIAN_POINT ( 'NONE',  ( -210.0000000000000000, 19.40000000000000213, 0.000000000000000000 ) ) ;
#11598 = SHAPE_DEFINITION_REPRESENTATION ( #6794, #8443 ) ;
#11599 = ADVANCED_FACE ( 'NONE', ( #719 ), #7640, .T. ) ;
#11600 = CARTESIAN_POINT ( 'NONE',  ( 0.000000000000000000, 19.00000000000000000, 208.0000000000000000 ) ) ;
#11601 = AXIS2_PLACEMENT_3D ( 'NONE', #9207, #83, #12342 ) ;
#11602 = ITEM_DEFINED_TRANSFORMATION ( 'NONE', 'NONE', #3401,  #805 ) ;
#11603 = CARTESIAN_POINT ( 'NONE',  ( -122.2593324768359935, 30.00000000000000000, -168.2755348299880040 ) ) ;
#11604 = ORIENTED_EDGE ( 'NONE', *, *, #1008, .T. ) ;
#11605 = CARTESIAN_POINT ( 'NONE',  ( -34.18476129325013346, 19.96883746093702428, -259.4723857429224267 ) ) ;
#11606 = DIRECTION ( 'NONE',  ( 0.000000000000000000, -1.000000000000000000, 0.000000000000000000 ) ) ;
#11607 = DIRECTION ( 'NONE',  ( -0.6368676505102696117, 0.000000000000000000, -0.7709731485165545184 ) ) ;
#11608 = CARTESIAN_POINT ( 'NONE',  ( 224.4939760857161843, -6.051844909775672576, 0.1192985195352710553 ) ) ;
#11609 = AXIS2_PLACEMENT_3D ( 'NONE', #3201, #6287, #11346 ) ;
#11610 = CARTESIAN_POINT ( 'NONE',  ( -246.8597181602070236, 20.08915143297737060, -83.79436865282342239 ) ) ;
#11611 = DIRECTION ( 'NONE',  ( 0.000000000000000000, -1.000000000000000000, 0.000000000000000000 ) ) ;
#11612 = CARTESIAN_POINT ( 'NONE',  ( -36.24423871767982774, -138.4705547276867321, 20.92562098022539629 ) ) ;
#11613 = ADVANCED_FACE ( 'NONE', ( #4904 ), #2952, .F. ) ;
#11614 = CARTESIAN_POINT ( 'NONE',  ( 0.000000000000000000, 11.79660968244693997, 0.000000000000000000 ) ) ;
#11615 = EDGE_CURVE ( 'NONE', #9653, #12948, #9139, .T. ) ;
#11616 = LINE ( 'NONE', #4531, #7038 ) ;
#11617 = PRESENTATION_LAYER_ASSIGNMENT (  '', '', ( #12459 ) ) ;
#11618 = CIRCLE ( 'NONE', #2247, 249.7999999999999829 ) ;
#11619 = CARTESIAN_POINT ( 'NONE',  ( -0.000000000000000000, -29.00000000000000000, 0.000000000000000000 ) ) ;
#11620 = ORIENTED_EDGE ( 'NONE', *, *, #5568, .T. ) ;
#11621 = EDGE_LOOP ( 'NONE', ( #6041, #1528 ) ) ;
#11622 = CARTESIAN_POINT ( 'NONE',  ( -287.1814104624966149, -30.00000000000000000, -23.44910453727290545 ) ) ;
#11623 = DIRECTION ( 'NONE',  ( -0.6368676505102689456, 0.000000000000000000, -0.7709731485165549625 ) ) ;
#11624 = CARTESIAN_POINT ( 'NONE',  ( -115.8123742913374770, 20.55460285152583921, -234.8993005728878529 ) ) ;
#11625 = AXIS2_PLACEMENT_3D ( 'NONE', #3443, #10583, #1452 ) ;
#11626 = FACE_OUTER_BOUND ( 'NONE', #2080, .T. ) ;
#11627 =( REPRESENTATION_RELATIONSHIP ('NONE','NONE', #12019, #11671 ) REPRESENTATION_RELATIONSHIP_WITH_TRANSFORMATION ( #2765 )SHAPE_REPRESENTATION_RELATIONSHIP( ) );
#11628 = CARTESIAN_POINT ( 'NONE',  ( 0.000000000000000000, 0.000000000000000000, 0.000000000000000000 ) ) ;
#11629 = DIRECTION ( 'NONE',  ( 0.000000000000000000, 0.000000000000000000, -1.000000000000000000 ) ) ;
#11630 = CARTESIAN_POINT ( 'NONE',  ( -247.0684411393755795, 20.79694577634646535, -83.86521783953202203 ) ) ;
#11631 = CIRCLE ( 'NONE', #5880, 6.500000000000005329 ) ;
#11632 = EDGE_CURVE ( 'NONE', #1648, #7179, #4246, .T. ) ;
#11633 = ORIENTED_EDGE ( 'NONE', *, *, #11459, .T. ) ;
#11634 = CARTESIAN_POINT ( 'NONE',  ( 17.06764083276477706, 20.79694577634646890, -260.3553053170167004 ) ) ;
#11635 = ORIENTED_EDGE ( 'NONE', *, *, #8459, .F. ) ;
#11636 = DIRECTION ( 'NONE',  ( -0.000000000000000000, -1.000000000000000000, 0.000000000000000000 ) ) ;
#11637 = ORIENTED_EDGE ( 'NONE', *, *, #6859, .T. ) ;
#11638 = EDGE_LOOP ( 'NONE', ( #3832, #1268, #750, #55 ) ) ;
#11639 = DIRECTION ( 'NONE',  ( 0.000000000000000000, 0.000000000000000000, 1.000000000000000000 ) ) ;
#11640 = FACE_OUTER_BOUND ( 'NONE', #11135, .T. ) ;
#11641 = CARTESIAN_POINT ( 'NONE',  ( 239.4717458111675228, 1.490203034907673807, -3.166904956765172141 ) ) ;
#11642 = FACE_OUTER_BOUND ( 'NONE', #2499, .T. ) ;
#11643 = CARTESIAN_POINT ( 'NONE',  ( -249.7834747117774157, 11.65132285575429982, -2.887446915690841109 ) ) ;
#11644 = CYLINDRICAL_SURFACE ( 'NONE', #9439, 5.099999999999993427 ) ;
#11645 = ORIENTED_EDGE ( 'NONE', *, *, #3460, .F. ) ;
#11646 = CARTESIAN_POINT ( 'NONE',  ( -238.8031819202592487, -0.6747694104200937515, 11.73074746694206283 ) ) ;
#11647 = ORIENTED_EDGE ( 'NONE', *, *, #11661, .T. ) ;
#11648 = PRODUCT_DEFINITION_SHAPE ( 'NONE', 'NONE',  #13168 ) ;
#11649 = CARTESIAN_POINT ( 'NONE',  ( -243.0711418334325629, 7.372150985330255146, -9.149572406936686164 ) ) ;
#11650 = CARTESIAN_POINT ( 'NONE',  ( 122.2593324768334071, 30.00000000000000000, -168.2755348299895104 ) ) ;
#11651 = B_SPLINE_CURVE_WITH_KNOTS ( 'NONE', 3,
 ( #2904, #5721, #792, #12855, #6734, #10988, #9781, #8858, #3721, #11856, #2703, #8726, #7851, #12919, #9710, #10852, #858, #3648, #5792, #5925, #4710, #6988, #1860, #1726, #9852, #732, #4782, #10784, #3919, #2772, #3780, #11923, #6861, #4641, #2841, #1596, #10919, #1796, #4847, #8925, #1655, #3850, #6928, #9990, #4916, #8991, #12053, #11539, #7719, #7993, #5657, #12784, #11801, #10172, #8261, #4247, #10312, #925, #3240, #8328, #12316, #5248, #1052, #7255, #7126, #5176, #4049, #10114, #11116, #1192, #12120, #6120, #12257, #11183, #8198, #2976, #2049, #988, #5041, #5775, #9115, #12386, #3108, #3978, #248, #1986, #9257, #8053, #5111, #3174, #11053, #9317, #4982, #1924, #5994, #11320, #6263, #2114, #2183 ),
 .UNSPECIFIED., .F., .F.,
 ( 4, 2, 2, 1, 1, 2, 2, 2, 2, 1, 1, 1, 2, 2, 2, 2, 1, 1, 1, 1, 2, 2, 2, 2, 1, 1, 1, 1, 2, 2, 2, 2, 2, 2, 1, 1, 1, 1, 2, 2, 2, 2, 1, 1, 1, 1, 2, 2, 2, 2, 1, 1, 1, 1, 2, 2, 2, 2, 1, 1, 2, 2, 4 ),
 ( 0.000000000000000000, 0.03125000000005733608, 0.04687500000008829742, 0.05468750000010186990, 0.05859375000010871165, 0.06054687500011050189, 0.06250000000011228518, 0.09375000000013149204, 0.1093750000001398603, 0.1171875000001438988, 0.1210937500001458555, 0.1230468750001459111, 0.1240234375001469658, 0.1250000000001480205, 0.1875000000001324496, 0.2187500000001246225, 0.2343750000001203482, 0.2421875000001185441, 0.2460937500001179057, 0.2480468750001177947, 0.2490234375001177114, 0.2500000000001176281, 0.3125000000001167400, 0.3437500000001161293, 0.3593750000001158518, 0.3671875000001156297, 0.3710937500001154077, 0.3730468750001152967, 0.3740234375001151856, 0.3750000000001150746, 0.4375000000001111333, 0.5000000000001071365, 0.5625000000001032507, 0.5937500000001012523, 0.6093750000001003642, 0.6171875000000999201, 0.6210937500000995870, 0.6230468750000994760, 0.6240234375000994760, 0.6250000000000993650, 0.6875000000000954792, 0.7187500000000934808, 0.7343750000000922595, 0.7421875000000917044, 0.7460937500000911493, 0.7480468750000904832, 0.7490234375000901501, 0.7500000000000898170, 0.8125000000000358602, 0.8437500000000095479, 0.8593749999999962252, 0.8671874999999906741, 0.8710937499999866773, 0.8730468749999857891, 0.8740234374999852340, 0.8749999999999846789, 0.9062499999999700240, 0.9218749999999626965, 0.9296874999999605871, 0.9335937499999594769, 0.9355468749999606981, 0.9374999999999619194, 1.000000000000000000 ),
 .UNSPECIFIED. ) ;
#11652 = DIRECTION ( 'NONE',  ( 0.000000000000000000, 0.000000000000000000, 1.000000000000000000 ) ) ;
#11653 = CARTESIAN_POINT ( 'NONE',  ( -5.000000000000000000, 0.000000000000000000, 250.0000000000000000 ) ) ;
#11654 = CIRCLE ( 'NONE', #12918, 5.500000000000007994 ) ;
#11655 = DIRECTION ( 'NONE',  ( -0.6368676505102707219, 0.000000000000000000, -0.7709731485165535192 ) ) ;
#11656 = CARTESIAN_POINT ( 'NONE',  ( -229.8594613498277397, 8.573669842083557313, 8.043715334378049420 ) ) ;
#11657 = CARTESIAN_POINT ( 'NONE',  ( -248.5207756069831930, -9.904443213030258875, 6.775263355895822848 ) ) ;
#11658 = AXIS2_PLACEMENT_3D ( 'NONE', #6000, #9926, #12994 ) ;
#11659 = CARTESIAN_POINT ( 'NONE',  ( 227.3999999999999773, 4.447920636657316074, -2.686261716586451520 ) ) ;
#11660 = APPLICATION_PROTOCOL_DEFINITION ( 'draft international standard', 'automotive_design', 1998, #472 ) ;
#11661 = EDGE_CURVE ( 'NONE', #9350, #12208, #11977, .T. ) ;
#11662 = CARTESIAN_POINT ( 'NONE',  ( -229.9968423840866478, 11.93955909105315705, -1.301722993638689596 ) ) ;
#11663 = EDGE_CURVE ( 'NONE', #12029, #12239, #7775, .T. ) ;
#11664 = ITEM_DEFINED_TRANSFORMATION ( 'NONE', 'NONE', #5543,  #805 ) ;
#11665 = ORIENTED_EDGE ( 'NONE', *, *, #2051, .F. ) ;
#11666 = CARTESIAN_POINT ( 'NONE',  ( -228.6269314446401211, -19.00000000000000000, 181.7250016321579835 ) ) ;
#11667 = ORIENTED_EDGE ( 'NONE', *, *, #11354, .F. ) ;
#11668 = AXIS2_PLACEMENT_3D ( 'NONE', #227, #1294, #5359 ) ;
#11669 = CARTESIAN_POINT ( 'NONE',  ( 17.09264059789564172, 19.96883746058902176, -261.1558126970361400 ) ) ;
#11670 = CARTESIAN_POINT ( 'NONE',  ( 290.6841825403032544, -30.00000000000000000, 27.68945685411186730 ) ) ;
#11671 = SHAPE_REPRESENTATION ( 'Slewing Ring High Pressure Lip Seals Top Bottom', ( #805 ), #2501 ) ;
#11672 = DIRECTION ( 'NONE',  ( 0.6368676505102716101, 0.000000000000000000, 0.7709731485165527420 ) ) ;
#11673 = DIRECTION ( 'NONE',  ( 0.000000000000000000, -1.000000000000000000, 0.000000000000000000 ) ) ;
#11674 = CARTESIAN_POINT ( 'NONE',  ( -237.4577367525706393, 20.08915143297736705, 107.5873595010535411 ) ) ;
#11675 = DIRECTION ( 'NONE',  ( 0.000000000000000000, 1.000000000000000000, 0.000000000000000000 ) ) ;
#11676 = DIRECTION ( 'NONE',  ( 0.6427876096865379196, 0.000000000000000000, 0.7660444431189792347 ) ) ;
#11677 = CARTESIAN_POINT ( 'NONE',  ( -229.8890080036733821, -9.338233916645270583, -7.173345918784452380 ) ) ;
#11678 = AXIS2_PLACEMENT_3D ( 'NONE', #813, #3810, #2930 ) ;
#11679 = CARTESIAN_POINT ( 'NONE',  ( -239.9450917581429792, -2.156506209390995021, -11.80463811257499884 ) ) ;
#11680 = LINE ( 'NONE', #3398, #8148 ) ;
#11681 = VERTEX_POINT ( 'NONE', #2828 ) ;
#11682 = VERTEX_POINT ( 'NONE', #5709 ) ;
#11683 = DIRECTION ( 'NONE',  ( -0.6368676505102707219, 0.000000000000000000, -0.7709731485165535192 ) ) ;
#11684 = DIRECTION ( 'NONE',  ( 0.000000000000000000, 0.000000000000000000, 1.000000000000000000 ) ) ;
#11685 = VECTOR ( 'NONE', #1159, 1000.000000000000000 ) ;
#11686 = VECTOR ( 'NONE', #4377, 1000.000000000000000 ) ;
#11687 = EDGE_CURVE ( 'NONE', #327, #10957, #10199, .T. ) ;
#11688 = AXIS2_PLACEMENT_3D ( 'NONE', #5612, #11820, #3474 ) ;
#11689 = AXIS2_PLACEMENT_3D ( 'NONE', #8397, #3371, #1449 ) ;
#11690 = EDGE_CURVE ( 'NONE', #7101, #808, #1480, .T. ) ;
#11691 = CARTESIAN_POINT ( 'NONE',  ( -84.02568524183371323, 20.79694577604410100, 247.4557548106605225 ) ) ;
#11692 = DIRECTION ( 'NONE',  ( 0.000000000000000000, 1.000000000000000000, 0.000000000000000000 ) ) ;
#11693 = CARTESIAN_POINT ( 'NONE',  ( 0.000000000000000000, 0.000000000000000000, 0.000000000000000000 ) ) ;
#11694 = CARTESIAN_POINT ( 'NONE',  ( -182.4625818711933221, -19.00000000000000000, -220.8838070499919013 ) ) ;
#11695 = AXIS2_PLACEMENT_3D ( 'NONE', #1599, #2709, #5865 ) ;
#11696 = DIRECTION ( 'NONE',  ( -0.6368676505102707219, 0.000000000000000000, -0.7709731485165535192 ) ) ;
#11697 = VERTEX_POINT ( 'NONE', #2635 ) ;
#11698 = DIRECTION ( 'NONE',  ( 1.000000000000000000, -0.000000000000000000, 0.000000000000000000 ) ) ;
#11700 = EDGE_LOOP ( 'NONE', ( #3883, #11767, #4176, #4783 ) ) ;
#11699 = CIRCLE ( 'NONE', #453, 250.7029414592220178 ) ;
#11701 = FACE_OUTER_BOUND ( 'NONE', #2276, .T. ) ;
#11702 = ORIENTED_EDGE ( 'NONE', *, *, #11157, .F. ) ;
#11703 = ORIENTED_EDGE ( 'NONE', *, *, #9370, .F. ) ;
#11704 = CIRCLE ( 'NONE', #11057, 250.7000000000000171 ) ;
#11705 = DIRECTION ( 'NONE',  ( 0.6368676505102716101, 0.000000000000000000, 0.7709731485165527420 ) ) ;
#11706 = ADVANCED_FACE ( 'NONE', ( #8777 ), #11906, .F. ) ;
#11707 = FACE_OUTER_BOUND ( 'NONE', #4949, .T. ) ;
#11708 = CARTESIAN_POINT ( 'NONE',  ( -226.1171533167550081, 20.08915143289658545, -130.5770120871825952 ) ) ;
#11709 = CARTESIAN_POINT ( 'NONE',  ( 235.4000000000000057, 0.000000000000000000, 0.000000000000000000 ) ) ;
#11710 = DIRECTION ( 'NONE',  ( 0.000000000000000000, -0.7071067811865489050, -0.7071067811865460184 ) ) ;
#11711 = EDGE_CURVE ( 'NONE', #2919, #3933, #10633, .T. ) ;
#11712 = CONTEXT_DEPENDENT_SHAPE_REPRESENTATION ( #11449, #11388 ) ;
#11713 = EDGE_LOOP ( 'NONE', ( #5989, #2643 ) ) ;
#11714 = CARTESIAN_POINT ( 'NONE',  ( -238.9237350116528660, -1.003861713588480420, 11.70704244028693886 ) ) ;
#11715 = VERTEX_POINT ( 'NONE', #582 ) ;
#11716 = CARTESIAN_POINT ( 'NONE',  ( -244.1571280506203152, 8.217568834458665705, -8.398466971310503126 ) ) ;
#11717 = CARTESIAN_POINT ( 'NONE',  ( 234.4000000000000057, 0.000000000000000000, 0.000000000000000000 ) ) ;
#11718 = AXIS2_PLACEMENT_3D ( 'NONE', #4650, #7595, #474 ) ;
#11719 = CYLINDRICAL_SURFACE ( 'NONE', #11065, 12.00000000000000000 ) ;
#11720 = CARTESIAN_POINT ( 'NONE',  ( 234.4000000000000057, -3.999223041228189057, 0.07883569311883592556 ) ) ;
#11721 = CARTESIAN_POINT ( 'NONE',  ( -249.7915528516605548, -11.82778639353378125, -2.343958593077331898 ) ) ;
#11722 = DIRECTION ( 'NONE',  ( 0.000000000000000000, 0.9998057603070481525, -0.01970892327970899874 ) ) ;
#11723 = CARTESIAN_POINT ( 'NONE',  ( -122.2593324768321992, 30.00000000000000000, 162.7755348299905052 ) ) ;
#11724 = FACE_OUTER_BOUND ( 'NONE', #8583, .T. ) ;
#11725 = ITEM_DEFINED_TRANSFORMATION ( 'NONE', 'NONE', #3564,  #805 ) ;
#11726 = DIRECTION ( 'NONE',  ( -0.000000000000000000, -1.000000000000000000, 0.000000000000000000 ) ) ;
#11728 = ORIENTED_EDGE ( 'NONE', *, *, #7250, .T. ) ;
#11727 = AXIS2_PLACEMENT_3D ( 'NONE', #4059, #5258, #10124 ) ;
#11729 = CARTESIAN_POINT ( 'NONE',  ( 135.8846079354933352, -19.40000000000000213, -256.1940150085812888 ) ) ;
#11730 = VERTEX_POINT ( 'NONE', #2573 ) ;
#11731 =( REPRESENTATION_RELATIONSHIP ('NONE','NONE', #12019, #5191 ) REPRESENTATION_RELATIONSHIP_WITH_TRANSFORMATION ( #12670 )SHAPE_REPRESENTATION_RELATIONSHIP( ) );
#11732 = CARTESIAN_POINT ( 'NONE',  ( -252.8031682270705289, 19.96883745940372279, 67.71318189758537187 ) ) ;
#11733 = CARTESIAN_POINT ( 'NONE',  ( -193.6077657551222728, -30.00000000000000000, -234.3758371490322645 ) ) ;
#11734 = FACE_BOUND ( 'NONE', #5553, .T. ) ;
#11735 = EDGE_CURVE ( 'NONE', #7466, #1872, #5497, .T. ) ;
#11736 = LINE ( 'NONE', #5598, #12139 ) ;
#11737 = EDGE_LOOP ( 'NONE', ( #7852, #3007, #7608, #7575 ) ) ;
#11738 = CARTESIAN_POINT ( 'NONE',  ( -122.2593324768321992, 19.00000000000000000, 168.2755348299905052 ) ) ;
#11739 = CARTESIAN_POINT ( 'NONE',  ( 226.7234983661818717, 0.000000000000000000, 0.000000000000000000 ) ) ;
#11740 = DIRECTION ( 'NONE',  ( -0.7071067811865413555, 0.000000000000000000, -0.7071067811865536790 ) ) ;
#11741 = CARTESIAN_POINT ( 'NONE',  ( 229.9983344328827286, 3.389070926892647773, 0.9034159009639075588 ) ) ;
#11742 = ITEM_DEFINED_TRANSFORMATION ( 'NONE', 'NONE', #10612,  #805 ) ;
#11743 = CIRCLE ( 'NONE', #3639, 5.100000000000017408 ) ;
#11744 = CARTESIAN_POINT ( 'NONE',  ( -240.0865915474315102, -2.714760371352697987, -11.69235895547828363 ) ) ;
#11745 = CONICAL_SURFACE ( 'NONE', #10880, 6.500000000000005329, 0.7853981633974617127 ) ;
#11746 = ORIENTED_EDGE ( 'NONE', *, *, #2467, .F. ) ;
#11747 = DIRECTION ( 'NONE',  ( 0.000000000000000000, 1.000000000000000000, 0.000000000000000000 ) ) ;
#11748 = ORIENTED_EDGE ( 'NONE', *, *, #775, .F. ) ;
#11749 = ORIENTED_EDGE ( 'NONE', *, *, #9220, .T. ) ;
#11750 = DIRECTION ( 'NONE',  ( -1.000000000000000000, 0.000000000000000000, 0.000000000000000000 ) ) ;
#11751 = LINE ( 'NONE', #5678, #11219 ) ;
#11752 = ADVANCED_BREP_SHAPE_REPRESENTATION ( '', ( #1525, #805 ), #391 ) ;
#11753 = ADVANCED_FACE ( 'NONE', ( #1848 ), #10906, .F. ) ;
#11754 = CARTESIAN_POINT ( 'NONE',  ( 34.20858920311310669, 20.55460285062568815, 259.6535381495587558 ) ) ;
#11755 = CARTESIAN_POINT ( 'NONE',  ( 0.000000000000000000, 0.000000000000000000, 0.000000000000000000 ) ) ;
#11756 =( REPRESENTATION_RELATIONSHIP ('NONE','NONE', #12019, #5191 ) REPRESENTATION_RELATIONSHIP_WITH_TRANSFORMATION ( #6598 )SHAPE_REPRESENTATION_RELATIONSHIP( ) );
#11757 = DIRECTION ( 'NONE',  ( 0.000000000000000000, 0.000000000000000000, -1.000000000000000000 ) ) ;
#11758 = AXIS2_PLACEMENT_3D ( 'NONE', #7309, #9105, #978 ) ;
#11759 = FACE_OUTER_BOUND ( 'NONE', #1083, .T. ) ;
#11760 = ORIENTED_EDGE ( 'NONE', *, *, #579, .F. ) ;
#11761 = EDGE_CURVE ( 'NONE', #3580, #7040, #12907, .T. ) ;
#11762 = DIRECTION ( 'NONE',  ( -0.000000000000000000, -1.000000000000000000, 0.000000000000000000 ) ) ;
#11763 = VERTEX_POINT ( 'NONE', #3766 ) ;
#11764 = ORIENTED_EDGE ( 'NONE', *, *, #607, .T. ) ;
#11765 = AXIS2_PLACEMENT_3D ( 'NONE', #76, #10325, #4131 ) ;
#11766 = CARTESIAN_POINT ( 'NONE',  ( 225.7689075324037162, 20.08915143297736705, 130.3442252640563481 ) ) ;
#11767 = ORIENTED_EDGE ( 'NONE', *, *, #11182, .F. ) ;
#11768 = PRODUCT_DEFINITION_SHAPE ( 'NONE', 'NONE',  #13135 ) ;
#11769 = VECTOR ( 'NONE', #965, 1000.000000000000000 ) ;
#11770 = CARTESIAN_POINT ( 'NONE',  ( 227.3999999999999773, 2.999417280921144346, -0.05912676983912699968 ) ) ;
#11771 = DIRECTION ( 'NONE',  ( -1.224646799147349509E-16, 0.000000000000000000, -1.000000000000000000 ) ) ;
#11772 = AXIS2_PLACEMENT_3D ( 'NONE', #5949, #5004, #9077 ) ;
#11773 = CARTESIAN_POINT ( 'NONE',  ( 115.4648407707963997, 20.08915143305429041, -234.1947771728865177 ) ) ;
#11774 = CARTESIAN_POINT ( 'NONE',  ( -249.7380656782619042, 10.65316887761970222, -5.649205583226009963 ) ) ;
#11775 = SURFACE_STYLE_USAGE ( .BOTH. , #3827 ) ;
#11776 = ORIENTED_EDGE ( 'NONE', *, *, #10434, .F. ) ;
#11777 = DIRECTION ( 'NONE',  ( 0.000000000000000000, 0.000000000000000000, 1.000000000000000000 ) ) ;
#11779 = EDGE_CURVE ( 'NONE', #2818, #12564, #5958, .T. ) ;
#11778 = AXIS2_PLACEMENT_3D ( 'NONE', #3264, #1409, #8415 ) ;
#11780 = ORIENTED_EDGE ( 'NONE', *, *, #8186, .T. ) ;
#11781 = EDGE_CURVE ( 'NONE', #8160, #10938, #2795, .T. ) ;
#11782 = CIRCLE ( 'NONE', #6033, 12.00000000000000000 ) ;
#11783 = DIRECTION ( 'NONE',  ( -0.000000000000000000, -1.000000000000000000, 0.000000000000000000 ) ) ;
#11784 = ORIENTED_EDGE ( 'NONE', *, *, #5957, .T. ) ;
#11785 = ADVANCED_FACE ( 'NONE', ( #5235 ), #6047, .T. ) ;
#11786 = DIRECTION ( 'NONE',  ( -0.000000000000000000, -1.000000000000000000, 0.000000000000000000 ) ) ;
#11787 = DIRECTION ( 'NONE',  ( 0.000000000000000000, 1.000000000000000000, 0.000000000000000000 ) ) ;
#11788 = DIRECTION ( 'NONE',  ( -0.000000000000000000, -1.000000000000000000, 0.000000000000000000 ) ) ;
#11789 = CIRCLE ( 'NONE', #3897, 5.500000000000015099 ) ;
#11790 = DIRECTION ( 'NONE',  ( 0.000000000000000000, 0.01970892327970899874, 0.9998057603070481525 ) ) ;
#11791 = VECTOR ( 'NONE', #8702, 1000.000000000000000 ) ;
#11792 = VECTOR ( 'NONE', #2609, 1000.000000000000114 ) ;
#11793 = DIRECTION ( 'NONE',  ( -0.000000000000000000, -1.000000000000000000, 0.000000000000000000 ) ) ;
#11794 = DIRECTION ( 'NONE',  ( 0.000000000000000000, 1.000000000000000000, 0.000000000000000000 ) ) ;
#11795 = CARTESIAN_POINT ( 'NONE',  ( -229.7511168103433477, 5.440903037008435916, 10.69724303830294865 ) ) ;
#11796 = ORIENTED_EDGE ( 'NONE', *, *, #8812, .F. ) ;
#11797 = ADVANCED_FACE ( 'NONE', ( #1911 ), #10103, .F. ) ;
#11798 = PRODUCT_DEFINITION_SHAPE ( 'NONE', 'NONE',  #11012 ) ;
#11799 = CIRCLE ( 'NONE', #10944, 3.000000000000000000 ) ;
#11800 = ORIENTED_EDGE ( 'NONE', *, *, #11525, .F. ) ;
#11801 = CARTESIAN_POINT ( 'NONE',  ( -249.7944461408548307, -11.69162236593179927, 1.179780703821899479 ) ) ;
#11802 = ORIENTED_EDGE ( 'NONE', *, *, #2529, .F. ) ;
#11803 = CIRCLE ( 'NONE', #3700, 2.749999999999999556 ) ;
#11804 = CARTESIAN_POINT ( 'NONE',  ( -159.4136521839998011, 20.55460285116278385, -207.7919029849606432 ) ) ;
#11805 = CARTESIAN_POINT ( 'NONE',  ( 235.4000000000000057, -3.999223041228192610, 0.07883569311883648068 ) ) ;
#11806 = CARTESIAN_POINT ( 'NONE',  ( 0.000000000000000000, -13.19999999999999929, 0.000000000000000000 ) ) ;
#11807 = CARTESIAN_POINT ( 'NONE',  ( -197.8197553893924976, 29.00000000000000000, -64.27553482998719403 ) ) ;
#11808 = DIRECTION ( 'NONE',  ( 0.6368676505102716101, 0.000000000000000000, 0.7709731485165527420 ) ) ;
#11809 = VECTOR ( 'NONE', #3260, 1000.000000000000000 ) ;
#11810 = DIRECTION ( 'NONE',  ( 0.6368676505102716101, 0.000000000000000000, 0.7709731485165527420 ) ) ;
#11811 = CARTESIAN_POINT ( 'NONE',  ( 24.00488622054110621, -138.4705547276867321, -34.28253040793644146 ) ) ;
#11812 = CARTESIAN_POINT ( 'NONE',  ( 229.9799616755531133, 1.752001039403962013, -3.038685965070802908 ) ) ;
#11813 = ITEM_DEFINED_TRANSFORMATION ( 'NONE', 'NONE', #11510,  #805 ) ;
#11814 = CARTESIAN_POINT ( 'NONE',  ( -249.7838850256576393, 11.60404975224821911, 1.846229155174516023 ) ) ;
#11815 = CARTESIAN_POINT ( 'NONE',  ( -241.8394219704672423, -6.081466909965556944, -10.34544425870726592 ) ) ;
#11816 = CARTESIAN_POINT ( 'NONE',  ( -229.9812292664173015, -11.63484992564693599, 2.943925132602736028 ) ) ;
#11817 = VERTEX_POINT ( 'NONE', #12104 ) ;
#11818 = ORIENTED_EDGE ( 'NONE', *, *, #4920, .F. ) ;
#11819 = AXIS2_PLACEMENT_3D ( 'NONE', #3053, #2124, #9329 ) ;
#11820 = DIRECTION ( 'NONE',  ( 0.000000000000000000, 1.000000000000000000, 0.000000000000000000 ) ) ;
#11821 = FACE_BOUND ( 'NONE', #12094, .T. ) ;
#11822 = CARTESIAN_POINT ( 'NONE',  ( 115.8123742910162264, 20.55460285096275541, -234.8993005738286115 ) ) ;
#11823 = CARTESIAN_POINT ( 'NONE',  ( 0.000000000000000000, 0.000000000000000000, 0.000000000000000000 ) ) ;
#11824 = DIRECTION ( 'NONE',  ( 0.000000000000000000, 1.000000000000000000, 0.000000000000000000 ) ) ;
#11825 = LINE ( 'NONE', #561, #9488 ) ;
#11826 = AXIS2_PLACEMENT_3D ( 'NONE', #6996, #1998, #12998 ) ;
#11827 = ORIENTED_EDGE ( 'NONE', *, *, #2203, .F. ) ;
#11828 = EDGE_CURVE ( 'NONE', #900, #3975, #11487, .T. ) ;
#11829 = EDGE_CURVE ( 'NONE', #5993, #10052, #8182, .T. ) ;
#11830 = DIRECTION ( 'NONE',  ( 0.5469441386039890496, 0.000000000000000000, -0.8371691043312220470 ) ) ;
#11831 = EDGE_LOOP ( 'NONE', ( #9164, #4582, #5092, #3076 ) ) ;
#11832 = VERTEX_POINT ( 'NONE', #12043 ) ;
#11833 = CARTESIAN_POINT ( 'NONE',  ( 42.46883004693734875, 20.08915143297736350, 257.2112267038639288 ) ) ;
#11834 = EDGE_LOOP ( 'NONE', ( #10914, #5057, #12556, #3965 ) ) ;
#11835 = DIRECTION ( 'NONE',  ( 0.000000000000000000, 1.000000000000000000, 0.000000000000000000 ) ) ;
#11836 = DIRECTION ( 'NONE',  ( 0.000000000000000000, 0.000000000000000000, 1.000000000000000000 ) ) ;
#11837 = CARTESIAN_POINT ( 'NONE',  ( -247.2466869557850089, 20.08915143288961858, -83.95474316020511196 ) ) ;
#11838 = CARTESIAN_POINT ( 'NONE',  ( -122.2593324768359935, 19.00000000000000000, -173.7755348299880040 ) ) ;
#11839 = ORIENTED_EDGE ( 'NONE', *, *, #11419, .F. ) ;
#11840 = FACE_OUTER_BOUND ( 'NONE', #3060, .T. ) ;
#11841 = VERTEX_POINT ( 'NONE', #5980 ) ;
#11842 = CARTESIAN_POINT ( 'NONE',  ( -241.1122039833427380, 5.014049992556535607, -10.62747927431669837 ) ) ;
#11843 = ORIENTED_EDGE ( 'NONE', *, *, #3460, .T. ) ;
#11844 = CARTESIAN_POINT ( 'NONE',  ( 240.1928509381488368, -2.335100009099129181, -2.607195044886591706 ) ) ;
#11845 = LINE ( 'NONE', #7642, #5124 ) ;
#11846 = DIRECTION ( 'NONE',  ( 0.000000000000000000, -1.000000000000000000, 0.000000000000000000 ) ) ;
#11847 = EDGE_CURVE ( 'NONE', #10670, #9039, #10838, .T. ) ;
#11848 = DIRECTION ( 'NONE',  ( 0.000000000000000000, 0.000000000000000000, -1.000000000000000000 ) ) ;
#11849 = ADVANCED_FACE ( 'NONE', ( #4035 ), #49, .T. ) ;
#11850 = CARTESIAN_POINT ( 'NONE',  ( -240.9947549593328802, -4.840187565308244011, 10.98379185734033925 ) ) ;
#11851 = CARTESIAN_POINT ( 'NONE',  ( 227.3999999999999773, 0.000000000000000000, 0.000000000000000000 ) ) ;
#11852 = CONTEXT_DEPENDENT_SHAPE_REPRESENTATION ( #12981, #3183 ) ;
#11853 = VERTEX_POINT ( 'NONE', #3027 ) ;
#11854 = CARTESIAN_POINT ( 'NONE',  ( -229.8036261751163352, 7.330002591760357511, 9.502943147174924832 ) ) ;
#11855 = ORIENTED_EDGE ( 'NONE', *, *, #1769, .T. ) ;
#11856 = CARTESIAN_POINT ( 'NONE',  ( -248.8038635818411421, -10.11061836954485926, -5.986481948888957128 ) ) ;
#11857 = ORIENTED_EDGE ( 'NONE', *, *, #8934, .T. ) ;
#11858 = CARTESIAN_POINT ( 'NONE',  ( -84.20717312374198116, 20.55460285077014504, 247.9906035358103225 ) ) ;
#11859 = DIRECTION ( 'NONE',  ( 0.6368676505102707219, 0.000000000000000000, 0.7709731485165536302 ) ) ;
#11860 = DIRECTION ( 'NONE',  ( 0.000000000000000000, 0.000000000000000000, 1.000000000000000000 ) ) ;
#11861 = CARTESIAN_POINT ( 'NONE',  ( -197.8197553893909912, 30.00000000000000000, 70.77553482999131518 ) ) ;
#11862 = EDGE_CURVE ( 'NONE', #3549, #8633, #11699, .T. ) ;
#11863 = CARTESIAN_POINT ( 'NONE',  ( -241.2266029204368465, 5.216955500457195249, 10.80672559037492952 ) ) ;
#11864 = LINE ( 'NONE', #10596, #7073 ) ;
#11865 = DIRECTION ( 'NONE',  ( -0.9848077530122091305, 0.000000000000000000, 0.1736481776669241417 ) ) ;
#11866 = CARTESIAN_POINT ( 'NONE',  ( 229.9733680233430562, 0.2283798993542111577, -3.499999999999966693 ) ) ;
#11867 = EDGE_CURVE ( 'NONE', #9988, #6569, #9172, .T. ) ;
#11868 = ITEM_DEFINED_TRANSFORMATION ( 'NONE', 'NONE', #442,  #805 ) ;
#11869 = PRODUCT_DEFINITION_SHAPE ( 'NONE', 'NONE',  #13152 ) ;
#11870 = CARTESIAN_POINT ( 'NONE',  ( -249.7865125416454362, 11.62303781398087921, -1.723091324902960242 ) ) ;
#11871 = CARTESIAN_POINT ( 'NONE',  ( -242.2626230869292101, -6.580656946410289088, -10.03470782670428996 ) ) ;
#11872 = AXIS2_PLACEMENT_3D ( 'NONE', #11738, #8864, #7928 ) ;
#11873 =( REPRESENTATION_RELATIONSHIP ('NONE','NONE', #12019, #182 ) REPRESENTATION_RELATIONSHIP_WITH_TRANSFORMATION ( #5638 )SHAPE_REPRESENTATION_RELATIONSHIP( ) );
#11874 = CARTESIAN_POINT ( 'NONE',  ( -229.6989039822362599, -2.469951368212909060, -11.76658813962577277 ) ) ;
#11875 = ORIENTED_EDGE ( 'NONE', *, *, #12888, .F. ) ;
#11876 = ORIENTED_EDGE ( 'NONE', *, *, #218, .T. ) ;
#11877 = CARTESIAN_POINT ( 'NONE',  ( -67.55708173888510260, 20.08915143292433214, 252.2208631666720180 ) ) ;
#11878 = DIRECTION ( 'NONE',  ( 0.6368676505102706109, 0.000000000000000000, 0.7709731485165535192 ) ) ;
#11879 = CARTESIAN_POINT ( 'NONE',  ( 261.3381329044966606, 20.55460285106647689, 17.10461161501256555 ) ) ;
#11880 = DIRECTION ( 'NONE',  ( -0.9848077530122091305, 0.000000000000000000, 0.1736481776669241417 ) ) ;
#11881 = DIRECTION ( 'NONE',  ( 0.000000000000000000, -1.000000000000000000, 0.000000000000000000 ) ) ;
#11882 = CYLINDRICAL_SURFACE ( 'NONE', #10758, 5.499999999999986677 ) ;
#11883 = ORIENTED_EDGE ( 'NONE', *, *, #7831, .T. ) ;
#11884 = CARTESIAN_POINT ( 'NONE',  ( -238.7879693975320947, -0.6590516350396603551, 11.98189593670389463 ) ) ;
#11885 = ORIENTED_EDGE ( 'NONE', *, *, #1353, .F. ) ;
#11886 = ORIENTED_EDGE ( 'NONE', *, *, #3579, .F. ) ;
#11887 = AXIS2_PLACEMENT_3D ( 'NONE', #9601, #7550, #2542 ) ;
#11888 = AXIS2_PLACEMENT_3D ( 'NONE', #8011, #7011, #2133 ) ;
#11889 = AXIS2_PLACEMENT_3D ( 'NONE', #8083, #10336, #19 ) ;
#11890 = CARTESIAN_POINT ( 'NONE',  ( 239.9471905437635826, -1.993882481329591450, 2.878173188141093686 ) ) ;
#11891 = ORIENTED_EDGE ( 'NONE', *, *, #11761, .T. ) ;
#11892 = DIRECTION ( 'NONE',  ( 1.000000000000000000, 0.000000000000000000, 0.000000000000000000 ) ) ;
#11893 = EDGE_CURVE ( 'NONE', #12419, #237, #9355, .T. ) ;
#11894 = CARTESIAN_POINT ( 'NONE',  ( -172.1812796679919870, 20.08915143287683591, 196.2980642839890209 ) ) ;
#11895 = FACE_OUTER_BOUND ( 'NONE', #7548, .T. ) ;
#11896 = CARTESIAN_POINT ( 'NONE',  ( -247.4267604609593718, 9.686619269043202252, 6.650504617425251119 ) ) ;
#11897 = PRODUCT_DEFINITION_SHAPE ( 'NONE', 'NONE',  #13049 ) ;
#11898 = AXIS2_PLACEMENT_3D ( 'NONE', #862, #1730, #3652 ) ;
#11899 = ORIENTED_EDGE ( 'NONE', *, *, #3786, .F. ) ;
#11900 = CARTESIAN_POINT ( 'NONE',  ( 2.816687638038912194E-14, 18.00000000000000000, 230.0000000000000000 ) ) ;
#11901 = AXIS2_PLACEMENT_3D ( 'NONE', #11959, #3885, #12086 ) ;
#11902 = EDGE_LOOP ( 'NONE', ( #942, #4478, #6306, #4551 ) ) ;
#11903 = CARTESIAN_POINT ( 'NONE',  ( -247.6398763875693021, 9.748465891793076210, -6.561428695001272793 ) ) ;
#11904 = EDGE_LOOP ( 'NONE', ( #2164, #10340, #10565, #2284 ) ) ;
#11905 = AXIS2_PLACEMENT_3D ( 'NONE', #11729, #12526, #7394 ) ;
#11906 = CONICAL_SURFACE ( 'NONE', #5731, 5.500000000000005329, 0.7853981633974461696 ) ;
#11907 = DIRECTION ( 'NONE',  ( 0.000000000000000000, 1.000000000000000000, 0.000000000000000000 ) ) ;
#11908 = LINE ( 'NONE', #10159, #9400 ) ;
#11909 = DIRECTION ( 'NONE',  ( 0.000000000000000000, 0.000000000000000000, 1.000000000000000000 ) ) ;
#11910 = ADVANCED_FACE ( 'NONE', ( #11640 ), #842, .T. ) ;
#11911 = CARTESIAN_POINT ( 'NONE',  ( 0.000000000000000000, 0.000000000000000000, 0.000000000000000000 ) ) ;
#11912 = FACE_BOUND ( 'NONE', #10130, .T. ) ;
#11913 = CARTESIAN_POINT ( 'NONE',  ( -243.5181255321092522, -7.757956330428957159, 9.154932349471659236 ) ) ;
#11914 = CARTESIAN_POINT ( 'NONE',  ( -83.86521783953165254, 20.79694577634646535, -247.0684411393756363 ) ) ;
#11915 = VERTEX_POINT ( 'NONE', #1435 ) ;
#11916 = DIRECTION ( 'NONE',  ( 1.000000000000000000, 0.000000000000000000, 0.000000000000000000 ) ) ;
#11917 = CIRCLE ( 'NONE', #8946, 6.500000000000005329 ) ;
#11918 = ORIENTED_EDGE ( 'NONE', *, *, #8123, .F. ) ;
#11919 = ADVANCED_FACE ( 'NONE', ( #314 ), #11508, .F. ) ;
#11920 = CIRCLE ( 'NONE', #9794, 6.500000000000005329 ) ;
#11921 = VERTEX_POINT ( 'NONE', #10433 ) ;
#11922 = ADVANCED_FACE ( 'NONE', ( #175 ), #8572, .T. ) ;
#11923 = CARTESIAN_POINT ( 'NONE',  ( -249.6746543472006294, -11.17527903296180902, -3.629830555839320017 ) ) ;
#11924 = ORIENTED_EDGE ( 'NONE', *, *, #12335, .T. ) ;
#11925 = CARTESIAN_POINT ( 'NONE',  ( 159.4136521832723474, 20.55460285070720161, -207.7919029841772840 ) ) ;
#11926 = DIRECTION ( 'NONE',  ( 0.6368676505102707219, 0.000000000000000000, 0.7709731485165535192 ) ) ;
#11927 = DIRECTION ( 'NONE',  ( -0.6368676505102707219, 0.000000000000000000, -0.7709731485165535192 ) ) ;
#11928 = CARTESIAN_POINT ( 'NONE',  ( 0.000000000000000000, -22.00000000000000000, 0.000000000000000000 ) ) ;
#11929 = CARTESIAN_POINT ( 'NONE',  ( -242.2196200858086286, 6.532801875907670919, 10.06598912815299229 ) ) ;
#11930 = AXIS2_PLACEMENT_3D ( 'NONE', #8416, #4590, #2533 ) ;
#11931 = FILL_AREA_STYLE_COLOUR ( '', #761 ) ;
#11932 = DIRECTION ( 'NONE',  ( -0.9961946980917461003, 0.000000000000000000, 0.08715574274765156004 ) ) ;
#11933 = CARTESIAN_POINT ( 'NONE',  ( 229.9832377166102333, 2.139172145189874641, 2.779699421282463945 ) ) ;
#11934 = CONTEXT_DEPENDENT_SHAPE_REPRESENTATION ( #7216, #11131 ) ;
#11935 = CIRCLE ( 'NONE', #10866, 6.500000000000005329 ) ;
#11936 = CARTESIAN_POINT ( 'NONE',  ( -249.7846912503109422, 11.60973349265466581, -1.810138449587363807 ) ) ;
#11937 = EDGE_CURVE ( 'NONE', #5214, #3553, #3227, .T. ) ;
#11938 = CARTESIAN_POINT ( 'NONE',  ( -244.7822625619571681, -8.616351828212369668, -8.352152985936292851 ) ) ;
#11939 = EDGE_CURVE ( 'NONE', #12436, #9851, #11437, .T. ) ;
#11940 = CARTESIAN_POINT ( 'NONE',  ( -229.9990782680060306, -11.98248316673616110, -0.7483019246402946578 ) ) ;
#11941 = ORIENTED_EDGE ( 'NONE', *, *, #9465, .T. ) ;
#11942 = VERTEX_POINT ( 'NONE', #5439 ) ;
#11943 = CARTESIAN_POINT ( 'NONE',  ( -239.4550142755241779, -1.775421017243286492, -11.61532944342562956 ) ) ;
#11944 = CARTESIAN_POINT ( 'NONE',  ( 0.000000000000000000, -11.79660968244690089, 249.7999999999999829 ) ) ;
#11945 = DIRECTION ( 'NONE',  ( 0.000000000000000000, 1.000000000000000000, 0.000000000000000000 ) ) ;
#11946 = ADVANCED_FACE ( 'NONE', ( #7566 ), #8305, .F. ) ;
#11947 = CARTESIAN_POINT ( 'NONE',  ( -130.6873781513712061, 20.79694577639645203, -226.3083638771730079 ) ) ;
#11948 = CARTESIAN_POINT ( 'NONE',  ( 233.5975020798683204, 0.000000000000000000, 0.000000000000000000 ) ) ;
#11949 = DIRECTION ( 'NONE',  ( -0.6427876096865327016, 0.000000000000000000, -0.7660444431189835646 ) ) ;
#11950 = CARTESIAN_POINT ( 'NONE',  ( 229.9000000000000057, -4.550331206106116078, -2.508881407069070590 ) ) ;
#11951 = DIRECTION ( 'NONE',  ( 0.000000000000000000, 0.000000000000000000, -1.000000000000000000 ) ) ;
#11952 =( REPRESENTATION_RELATIONSHIP ('NONE','NONE', #12019, #5191 ) REPRESENTATION_RELATIONSHIP_WITH_TRANSFORMATION ( #6747 )SHAPE_REPRESENTATION_RELATIONSHIP( ) );
#11953 = PRODUCT_RELATED_PRODUCT_CATEGORY ( 'part', '', ( #4464 ) ) ;
#11954 = ORIENTED_EDGE ( 'NONE', *, *, #5384, .T. ) ;
#11955 = CARTESIAN_POINT ( 'NONE',  ( -239.6024283181542955, -1.916856350840707268, 11.84591042646273173 ) ) ;
#11956 = EDGE_LOOP ( 'NONE', ( #10803, #8436 ) ) ;
#11957 = EDGE_LOOP ( 'NONE', ( #7720, #3619, #12782, #10144 ) ) ;
#11958 = AXIS2_PLACEMENT_3D ( 'NONE', #5559, #12630, #4421 ) ;
#11959 = CARTESIAN_POINT ( 'NONE',  ( 0.000000000000000000, -11.79660968244690089, 0.000000000000000000 ) ) ;
#11960 = EDGE_LOOP ( 'NONE', ( #3156, #2811, #8230, #5436 ) ) ;
#11961 = DIRECTION ( 'NONE',  ( 0.000000000000000000, 1.000000000000000000, 0.000000000000000000 ) ) ;
#11962 = CIRCLE ( 'NONE', #285, 10.00000000000000178 ) ;
#11963 = CARTESIAN_POINT ( 'NONE',  ( 194.2446334056325554, -19.00000000000000000, 235.1468102975488250 ) ) ;
#11964 = CARTESIAN_POINT ( 'NONE',  ( -289.8128292627096130, -18.00000000000000000, 10.41748504886635907 ) ) ;
#11965 =( LENGTH_UNIT ( ) NAMED_UNIT ( * ) SI_UNIT ( .MILLI., .METRE. ) );
#11966 = ORIENTED_EDGE ( 'NONE', *, *, #3938, .F. ) ;
#11967 = CARTESIAN_POINT ( 'NONE',  ( -289.8128292627096130, -30.00000000000000000, 10.41748504886635907 ) ) ;
#11968 = AXIS2_PLACEMENT_3D ( 'NONE', #6750, #10869, #11067 ) ;
#11969 = ORIENTED_EDGE ( 'NONE', *, *, #10030, .F. ) ;
#11970 = CARTESIAN_POINT ( 'NONE',  ( -239.2756941055121445, 1.575846662935195042, 11.64383230858651075 ) ) ;
#11971 = ORIENTED_EDGE ( 'NONE', *, *, #10554, .F. ) ;
#11972 = CONICAL_SURFACE ( 'NONE', #7925, 6.500000000000005329, 0.7853981633974518317 ) ;
#11973 = ADVANCED_FACE ( 'NONE', ( #3292 ), #8709, .T. ) ;
#11974 = AXIS2_PLACEMENT_3D ( 'NONE', #3033, #3163, #10164 ) ;
#11975 = CARTESIAN_POINT ( 'NONE',  ( -159.3442861576697283, -29.00000000000000000, -192.8974817588416499 ) ) ;
#11976 = CARTESIAN_POINT ( 'NONE',  ( 159.6627199829248411, -25.00000000000000000, 193.2829683331000012 ) ) ;
#11977 = LINE ( 'NONE', #3836, #10413 ) ;
#11978 = DIRECTION ( 'NONE',  ( 0.000000000000000000, 0.000000000000000000, 1.000000000000000000 ) ) ;
#11979 = FACE_BOUND ( 'NONE', #6322, .T. ) ;
#11980 = PRODUCT_DEFINITION_SHAPE ( 'NONE', 'NONE',  #13133 ) ;
#11981 = CARTESIAN_POINT ( 'NONE',  ( -241.1422742072429628, -5.089614320943621095, 10.87069852631545963 ) ) ;
#11982 = AXIS2_PLACEMENT_3D ( 'NONE', #11143, #4276, #2013 ) ;
#11983 =( REPRESENTATION_RELATIONSHIP ('NONE','NONE', #12019, #5191 ) REPRESENTATION_RELATIONSHIP_WITH_TRANSFORMATION ( #4863 )SHAPE_REPRESENTATION_RELATIONSHIP( ) );
#11984 = CARTESIAN_POINT ( 'NONE',  ( -151.9741924115230347, 20.79694577634646535, -212.0849693193239602 ) ) ;
#11985 = CONTEXT_DEPENDENT_SHAPE_REPRESENTATION ( #10678, #9266 ) ;
#11986 = ORIENTED_EDGE ( 'NONE', *, *, #12177, .T. ) ;
#11987 = CIRCLE ( 'NONE', #5160, 6.500000000000005329 ) ;
#11988 = CARTESIAN_POINT ( 'NONE',  ( -130.7196491263533744, -20.00000000000000000, 200.0834159351620087 ) ) ;
#11989 = ORIENTED_EDGE ( 'NONE', *, *, #2230, .T. ) ;
#11990 = ADVANCED_FACE ( 'NONE', ( #3351 ), #7435, .T. ) ;
#11991 = EDGE_CURVE ( 'NONE', #2076, #3933, #8507, .T. ) ;
#11992 = VERTEX_POINT ( 'NONE', #12567 ) ;
#11993 = DIRECTION ( 'NONE',  ( 0.6368676505102707219, 0.000000000000000000, 0.7709731485165535192 ) ) ;
#11994 = ORIENTED_EDGE ( 'NONE', *, *, #7506, .F. ) ;
#11995 = AXIS2_PLACEMENT_3D ( 'NONE', #150, #12344, #211 ) ;
#11996 = AXIS2_PLACEMENT_3D ( 'NONE', #2292, #6377, #2430 ) ;
#11997 = CARTESIAN_POINT ( 'NONE',  ( -259.6535381484769118, 20.55460285079236016, -34.20858920326526942 ) ) ;
#11998 = CARTESIAN_POINT ( 'NONE',  ( -0.000000000000000000, -3.327561323230905366, 0.000000000000000000 ) ) ;
#11999 = CARTESIAN_POINT ( 'NONE',  ( 286.5445428119865028, -30.00000000000000000, 22.67813138875427015 ) ) ;
#12000 = AXIS2_PLACEMENT_3D ( 'NONE', #8369, #4410, #228 ) ;
#12001 = AXIS2_PLACEMENT_3D ( 'NONE', #8025, #4151, #11218 ) ;
#12002 = FACE_OUTER_BOUND ( 'NONE', #6860, .T. ) ;
#12003 = CARTESIAN_POINT ( 'NONE',  ( -122.2593324768321992, 18.00000000000000000, 174.7755348299905052 ) ) ;
#12004 = EDGE_CURVE ( 'NONE', #1170, #4419, #8089, .T. ) ;
#12005 =( NAMED_UNIT ( * ) PLANE_ANGLE_UNIT ( ) SI_UNIT ( $, .RADIAN. ) );
#12006 = DIRECTION ( 'NONE',  ( -0.8191520442889871356, 0.000000000000000000, -0.5735764363510527097 ) ) ;
#12007 = CARTESIAN_POINT ( 'NONE',  ( -229.9491826271834327, -10.71030805289945853, 4.847677504751631616 ) ) ;
#12008 = AXIS2_PLACEMENT_3D ( 'NONE', #9234, #4161, #9163 ) ;
#12009 = FACE_OUTER_BOUND ( 'NONE', #695, .T. ) ;
#12010 = ORIENTED_EDGE ( 'NONE', *, *, #12791, .T. ) ;
#12011 = ORIENTED_EDGE ( 'NONE', *, *, #2934, .F. ) ;
#12012 = DIRECTION ( 'NONE',  ( 0.000000000000000000, 0.000000000000000000, -1.000000000000000000 ) ) ;
#12013 = DIRECTION ( 'NONE',  ( -1.000000000000000000, 0.000000000000000000, 0.000000000000000000 ) ) ;
#12014 = CONICAL_SURFACE ( 'NONE', #11601, 270.0000000000000000, 0.7853981633974476129 ) ;
#12015 = EDGE_CURVE ( 'NONE', #6924, #4498, #2335, .T. ) ;
#12016 = CARTESIAN_POINT ( 'NONE',  ( 130.6873781525580114, 20.79694577610125705, 226.3083638772055224 ) ) ;
#12017 = EDGE_CURVE ( 'NONE', #11365, #7406, #9363, .T. ) ;
#12018 = FACE_OUTER_BOUND ( 'NONE', #5715, .T. ) ;
#12019 = SHAPE_REPRESENTATION ( 'MAS-489', ( #10661, #9109, #7827, #6135, #12090, #8900, #11458, #9733, #3142, #3564, #12309, #4206, #3349, #10600, #2917, #4849, #4420, #11236, #11668, #2291, #8048, #6349, #12520, #6777, #8480, #2706, #399, #12728, #8285, #4000, #8491, #11028, #1459, #5503, #12097, #3573, #11463, #4429, #7210, #6358, #9539, #9331, #6786, #2521, #5711, #8272, #7626, #1032, #8689, #2510, #1878, #11678, #9742, #3152, #5282, #4632, #606, #8056, #2717, #1667, #5065, #2928, #12323, #10388, #5927, #12953, #2301, #6990, #2358, #11889, #8913, #7416, #3796, #1242, #3358, #9965, #4214, #10176, #9118, #6146, #7839, #10818, #10612, #12525, #2093, #11252, #4864, #6581, #825, #181, #11930, #5978, #10017, #6190, #229, #1071, #2349, #8327, #7464, #2984, #442, #7042, #5756, #9385, #7673, #6825, #11510, #7881, #12364, #1932, #8532, #4266, #4048, #11295, #2975, #12143, #3192, #9790, #6618, #2560, #16, #647, #12997, #2136, #1711, #10859, #866, #4468, #9581, #10437, #9161, #1501, #3401, #4676, #5109, #6403, #3834, #11084, #12571, #2756, #10222, #11727, #5543, #7254, #8955, #10448, #5337, #3624, #1296, #12781, #10653 ), #12580 ) ;
#12020 = DIRECTION ( 'NONE',  ( 0.2588190451025280669, 0.000000000000000000, -0.9659258262890663138 ) ) ;
#12021 = CARTESIAN_POINT ( 'NONE',  ( -243.8540711424298024, -8.004651151255652408, 8.601279216952042006 ) ) ;
#12022 = ORIENTED_EDGE ( 'NONE', *, *, #12557, .T. ) ;
#12023 = DIRECTION ( 'NONE',  ( -0.4503334343941562956, 0.7071067811865480168, -0.5451603414287978788 ) ) ;
#12024 = CIRCLE ( 'NONE', #11609, 6.500000000000000000 ) ;
#12025 = CARTESIAN_POINT ( 'NONE',  ( -239.4341775679679643, -1.763735199333067882, 11.86967692310885347 ) ) ;
#12026 = ORIENTED_EDGE ( 'NONE', *, *, #1466, .F. ) ;
#12027 = VERTEX_POINT ( 'NONE', #6314 ) ;
#12028 = DIRECTION ( 'NONE',  ( 0.000000000000000000, 0.9998057603070481525, -0.01970892327970900221 ) ) ;
#12029 = VERTEX_POINT ( 'NONE', #9500 ) ;
#12030 = CARTESIAN_POINT ( 'NONE',  ( -249.6197023356864406, 11.04161720034240268, 4.018949318582678565 ) ) ;
#12031 = CARTESIAN_POINT ( 'NONE',  ( -34.18476129325013346, 19.96883746093702428, -259.4723857429224267 ) ) ;
#12032 = EDGE_CURVE ( 'NONE', #3236, #1725, #12374, .T. ) ;
#12033 = CARTESIAN_POINT ( 'NONE',  ( 31.19222893192146273, -19.00000000000000000, -286.4438302234615890 ) ) ;
#12034 = EDGE_LOOP ( 'NONE', ( #4160, #110, #8564, #11796 ) ) ;
#12035 = DIRECTION ( 'NONE',  ( 0.000000000000000000, 0.000000000000000000, -1.000000000000000000 ) ) ;
#12036 = ORIENTED_EDGE ( 'NONE', *, *, #2205, .F. ) ;
#12037 = CARTESIAN_POINT ( 'NONE',  ( -239.2060324291192615, 1.486384971936542065, 11.65560575465026538 ) ) ;
#12038 = ORIENTED_EDGE ( 'NONE', *, *, #10308, .F. ) ;
#12039 = VECTOR ( 'NONE', #9492, 1000.000000000000000 ) ;
#12040 = AXIS2_PLACEMENT_3D ( 'NONE', #2095, #6437, #9367 ) ;
#12041 = CARTESIAN_POINT ( 'NONE',  ( 31.19222893192146273, -30.00000000000000000, -286.4438302234615890 ) ) ;
#12042 = CARTESIAN_POINT ( 'NONE',  ( 240.3318468625426476, 2.620158398681741829, 2.323190430345948521 ) ) ;
#12043 = CARTESIAN_POINT ( 'NONE',  ( 131.7449682071765835, -30.00000000000000000, -261.2053404739389180 ) ) ;
#12044 = CARTESIAN_POINT ( 'NONE',  ( -229.9960196359727433, 11.67278588814162532, 1.547559380408666252 ) ) ;
#12045 = CARTESIAN_POINT ( 'NONE',  ( 139.1326329530957082, -19.40000000000000213, -252.2620519511468729 ) ) ;
#12046 = CARTESIAN_POINT ( 'NONE',  ( -244.1511139035978317, -8.221670795503211338, 8.740858670380884377 ) ) ;
#12047 = AXIS2_PLACEMENT_3D ( 'NONE', #2270, #3266, #10403 ) ;
#12048 = CARTESIAN_POINT ( 'NONE',  ( -239.6024283463667075, 1.916856374241466821, -11.84591042273142669 ) ) ;
#12049 = ORIENTED_EDGE ( 'NONE', *, *, #10487, .T. ) ;
#12050 = CARTESIAN_POINT ( 'NONE',  ( -238.9707249641996611, -1.103996724206196323, -11.69802420276602462 ) ) ;
#12051 = ORIENTED_EDGE ( 'NONE', *, *, #11390, .F. ) ;
#12052 = EDGE_LOOP ( 'NONE', ( #10095, #3843 ) ) ;
#12053 = CARTESIAN_POINT ( 'NONE',  ( -249.7894049738271178, -11.64306034850750571, -1.598052574140636839 ) ) ;
#12054 = EDGE_LOOP ( 'NONE', ( #1098, #8657, #4485, #3280 ) ) ;
#12055 = CARTESIAN_POINT ( 'NONE',  ( -234.8993005728878529, 20.55460285095910677, 115.8123742916932741 ) ) ;
#12056 = CARTESIAN_POINT ( 'NONE',  ( -248.0636855450023575, 9.829232303934618997, -6.883789224338879187 ) ) ;
#12057 = DIRECTION ( 'NONE',  ( 0.6368676505102709440, 0.000000000000000000, 0.7709731485165532971 ) ) ;
#12058 = EDGE_CURVE ( 'NONE', #12948, #9653, #4663, .T. ) ;
#12059 = CARTESIAN_POINT ( 'NONE',  ( -244.2419534947191551, 8.283406883053094916, 8.682674417521349497 ) ) ;
#12060 =( REPRESENTATION_RELATIONSHIP ('NONE','NONE', #12019, #5191 ) REPRESENTATION_RELATIONSHIP_WITH_TRANSFORMATION ( #7217 )SHAPE_REPRESENTATION_RELATIONSHIP( ) );
#12061 = EDGE_CURVE ( 'NONE', #2233, #8497, #5531, .T. ) ;
#12062 = DIRECTION ( 'NONE',  ( 0.6368676505102737195, 0.000000000000000000, 0.7709731485165509657 ) ) ;
#12063 = DIRECTION ( 'NONE',  ( 0.7660444431189857850, 0.000000000000000000, -0.6427876096865300370 ) ) ;
#12064 = DIRECTION ( 'NONE',  ( -0.000000000000000000, -1.000000000000000000, 0.000000000000000000 ) ) ;
#12065 = ADVANCED_BREP_SHAPE_REPRESENTATION ( '', ( #5959, #805 ), #1235 ) ;
#12066 = CARTESIAN_POINT ( 'NONE',  ( -250.0000000000000000, -1.000000000000000000, 11.95826074310140008 ) ) ;
#12067 = ORIENTED_EDGE ( 'NONE', *, *, #9538, .T. ) ;
#12068 = ORIENTED_EDGE ( 'NONE', *, *, #4393, .F. ) ;
#12069 = PRODUCT_DEFINITION ( 'UNKNOWN', '', #5552, #292 ) ;
#12070 = CARTESIAN_POINT ( 'NONE',  ( 226.7234983661818717, 0.000000000000000000, 0.000000000000000000 ) ) ;
#12071 = CARTESIAN_POINT ( 'NONE',  ( 227.3999999999999773, 4.447920636657316074, -2.686261716586451520 ) ) ;
#12072 = CARTESIAN_POINT ( 'NONE',  ( 239.0740262672602796, -0.7008254641704574350, -3.430151065624111428 ) ) ;
#12073 = CARTESIAN_POINT ( 'NONE',  ( 159.0697709834164755, 20.79694577659177313, 207.3438552932204857 ) ) ;
#12074 = CARTESIAN_POINT ( 'NONE',  ( -193.6077657551223012, -18.00000000000000000, -234.3758371490321792 ) ) ;
#12075 = CARTESIAN_POINT ( 'NONE',  ( 0.000000000000000000, 0.000000000000000000, 0.000000000000000000 ) ) ;
#12076 = DIRECTION ( 'NONE',  ( 0.6368676505102716101, 0.000000000000000000, 0.7709731485165527420 ) ) ;
#12077 = CONTEXT_DEPENDENT_SHAPE_REPRESENTATION ( #1647, #6167 ) ;
#12078 = CIRCLE ( 'NONE', #11447, 251.8333333333380608 ) ;
#12079 = ORIENTED_EDGE ( 'NONE', *, *, #8928, .F. ) ;
#12080 = CARTESIAN_POINT ( 'NONE',  ( 3.034674768287141263E-14, 11.79660968244690089, -247.7999999999999829 ) ) ;
#12081 = DIRECTION ( 'NONE',  ( 0.000000000000000000, 1.000000000000000000, 0.000000000000000000 ) ) ;
#12082 = ORIENTED_EDGE ( 'NONE', *, *, #6243, .F. ) ;
#12083 = ORIENTED_EDGE ( 'NONE', *, *, #12898, .T. ) ;
#12084 = EDGE_CURVE ( 'NONE', #10637, #9436, #4032, .T. ) ;
#12085 = EDGE_CURVE ( 'NONE', #926, #8770, #3622, .T. ) ;
#12086 = DIRECTION ( 'NONE',  ( 0.000000000000000000, 0.000000000000000000, 1.000000000000000000 ) ) ;
#12087 = ORIENTED_EDGE ( 'NONE', *, *, #11939, .F. ) ;
#12088 = PRODUCT_DEFINITION_SHAPE ( 'NONE', 'NONE',  #13105 ) ;
#12089 = CARTESIAN_POINT ( 'NONE',  ( -248.8038635818159889, 10.11061836954053739, 5.986481948896264171 ) ) ;
#12090 = AXIS2_PLACEMENT_3D ( 'NONE', #7294, #12161, #4286 ) ;
#12091 = CARTESIAN_POINT ( 'NONE',  ( 247.2466869557899827, 20.08915143289970473, -83.95474316006121285 ) ) ;
#12092 = DIRECTION ( 'NONE',  ( 0.000000000000000000, 0.000000000000000000, -1.000000000000000000 ) ) ;
#12093 = CARTESIAN_POINT ( 'NONE',  ( -244.2656328542583424, 8.290010952302944602, 8.326962424296340259 ) ) ;
#12094 = EDGE_LOOP ( 'NONE', ( #1095, #3003 ) ) ;
#12095 = CARTESIAN_POINT ( 'NONE',  ( 0.000000000000000000, 24.99999999999995737, 0.000000000000000000 ) ) ;
#12096 = VECTOR ( 'NONE', #2411, 1000.000000000000114 ) ;
#12098 = EDGE_LOOP ( 'NONE', ( #12620, #10508, #4965, #10228 ) ) ;
#12097 = AXIS2_PLACEMENT_3D ( 'NONE', #9542, #9675, #559 ) ;
#12099 = CARTESIAN_POINT ( 'NONE',  ( -246.6344430665329810, 9.451372532324468168, -6.980988235906895767 ) ) ;
#12100 = ORIENTED_EDGE ( 'NONE', *, *, #2786, .F. ) ;
#12101 = EDGE_CURVE ( 'NONE', #11051, #3781, #12352, .T. ) ;
#12102 = DIRECTION ( 'NONE',  ( 0.000000000000000000, 0.000000000000000000, 1.000000000000000000 ) ) ;
#12103 = CARTESIAN_POINT ( 'NONE',  ( 239.9543636724889382, 1.989473563526599875, 2.884354563413217942 ) ) ;
#12104 = CARTESIAN_POINT ( 'NONE',  ( 159.3442861576696998, 19.00000000000000000, 192.8974817588417352 ) ) ;
#12105 = CIRCLE ( 'NONE', #5938, 6.500000000000005329 ) ;
#12106 = CARTESIAN_POINT ( 'NONE',  ( 0.000000000000000000, 30.00000000000000000, -208.0000000000000000 ) ) ;
#12107 = ADVANCED_FACE ( 'NONE', ( #11707 ), #1699, .F. ) ;
#12108 = AXIS2_PLACEMENT_3D ( 'NONE', #8862, #7791, #11860 ) ;
#12109 = CARTESIAN_POINT ( 'NONE',  ( -34.02434144668546168, 20.08915143297736705, -258.4638482596386098 ) ) ;
#12110 = VECTOR ( 'NONE', #6762, 1000.000000000000000 ) ;
#12111 = FACE_OUTER_BOUND ( 'NONE', #1727, .T. ) ;
#12112 = AXIS2_PLACEMENT_3D ( 'NONE', #8162, #10213, #11422 ) ;
#12113 = CARTESIAN_POINT ( 'NONE',  ( -42.50473797389721398, 20.79694577634646535, -257.4287020129719963 ) ) ;
#12114 = UNCERTAINTY_MEASURE_WITH_UNIT (LENGTH_MEASURE( 1.000000000000000082E-05 ), #4426, 'distance_accuracy_value', 'NONE');
#12115 = ORIENTED_EDGE ( 'NONE', *, *, #1916, .T. ) ;
#12116 = CIRCLE ( 'NONE', #5945, 5.499999999999998224 ) ;
#12117 = CARTESIAN_POINT ( 'NONE',  ( -239.2756941175678662, -1.575846677702103404, -11.64383230647870882 ) ) ;
#12118 = VECTOR ( 'NONE', #2457, 1000.000000000000000 ) ;
#12119 = VERTEX_POINT ( 'NONE', #7628 ) ;
#12120 = CARTESIAN_POINT ( 'NONE',  ( -249.6805863676327135, -11.19144319997654691, 3.579693128109238121 ) ) ;
#12121 = ORIENTED_EDGE ( 'NONE', *, *, #5468, .T. ) ;
#12122 = CARTESIAN_POINT ( 'NONE',  ( 226.3083638770190191, 20.79694577655596888, 130.6873781509345918 ) ) ;
#12123 = DIRECTION ( 'NONE',  ( 0.000000000000000000, 0.000000000000000000, -1.000000000000000000 ) ) ;
#12124 = CIRCLE ( 'NONE', #8299, 5.500000000000005329 ) ;
#12125 = DIRECTION ( 'NONE',  ( 1.000000000000000000, 0.000000000000000000, 0.000000000000000000 ) ) ;
#12126 = CARTESIAN_POINT ( 'NONE',  ( -241.6806182408534198, -5.858727366165308759, -10.18566440464593192 ) ) ;
#12127 =( REPRESENTATION_RELATIONSHIP ('NONE','NONE', #12019, #12521 ) REPRESENTATION_RELATIONSHIP_WITH_TRANSFORMATION ( #6853 )SHAPE_REPRESENTATION_RELATIONSHIP( ) );
#12128 = CARTESIAN_POINT ( 'NONE',  ( -249.7601711286373529, 11.14534860556848983, 4.601188512082746485 ) ) ;
#12129 = AXIS2_PLACEMENT_3D ( 'NONE', #2925, #4615, #12758 ) ;
#12130 = CARTESIAN_POINT ( 'NONE',  ( 239.7985776503645354, -1.848645179573700004, 2.971954070984049956 ) ) ;
#12131 = CARTESIAN_POINT ( 'NONE',  ( 41.69198534955607727, -138.4705547276867321, -3.647576077974657771 ) ) ;
#12132 = CARTESIAN_POINT ( 'NONE',  ( -229.7187050399571149, -3.051684812259986224, 11.37273813590071114 ) ) ;
#12133 = CIRCLE ( 'NONE', #2965, 248.1666666666679930 ) ;
#12134 = ITEM_DEFINED_TRANSFORMATION ( 'NONE', 'NONE', #1711,  #805 ) ;
#12135 = CYLINDRICAL_SURFACE ( 'NONE', #11765, 254.0000000000000000 ) ;
#12136 = EDGE_LOOP ( 'NONE', ( #2348, #8091, #5122, #12754, #11760, #11665 ) ) ;
#12137 = ORIENTED_EDGE ( 'NONE', *, *, #6654, .T. ) ;
#12138 = ADVANCED_FACE ( 'NONE', ( #8636 ), #12984, .F. ) ;
#12139 = VECTOR ( 'NONE', #4587, 1000.000000000000000 ) ;
#12140 = DIRECTION ( 'NONE',  ( 0.6368676505102707219, 0.000000000000000000, 0.7709731485165535192 ) ) ;
#12141 = CARTESIAN_POINT ( 'NONE',  ( -160.6180214586902650, -11.79660968244695951, -194.4394280558747710 ) ) ;
#12142 = CARTESIAN_POINT ( 'NONE',  ( -122.2593324768359935, 19.00000000000000000, -173.7755348299880040 ) ) ;
#12143 = AXIS2_PLACEMENT_3D ( 'NONE', #671, #10734, #2782 ) ;
#12144 = CARTESIAN_POINT ( 'NONE',  ( 5.000000000000000000, 0.000000000000000000, 250.0000000000000000 ) ) ;
#12145 = DIRECTION ( 'NONE',  ( -0.000000000000000000, -1.000000000000000000, 0.000000000000000000 ) ) ;
#12146 = CARTESIAN_POINT ( 'NONE',  ( 0.000000000000000000, 0.000000000000000000, 0.000000000000000000 ) ) ;
#12147 = AXIS2_PLACEMENT_3D ( 'NONE', #10310, #1191, #5246 ) ;
#12148 = CARTESIAN_POINT ( 'NONE',  ( -241.1122039834657471, -5.014049992762013019, 10.62747927426260830 ) ) ;
#12149 = ORIENTED_EDGE ( 'NONE', *, *, #10882, .F. ) ;
#12150 = FACE_OUTER_BOUND ( 'NONE', #12902, .T. ) ;
#12151 = EDGE_LOOP ( 'NONE', ( #11480, #10804, #8881, #10344 ) ) ;
#12152 = CARTESIAN_POINT ( 'NONE',  ( -238.8461604298144607, -0.8432863431609350924, 11.97040126094618273 ) ) ;
#12153 = ORIENTED_EDGE ( 'NONE', *, *, #4288, .T. ) ;
#12154 = EDGE_LOOP ( 'NONE', ( #841, #2770, #1566, #2677 ) ) ;
#12155 = LINE ( 'NONE', #7026, #1043 ) ;
#12156 = EDGE_LOOP ( 'NONE', ( #6077, #12856, #6645, #4596 ) ) ;
#12157 = DIRECTION ( 'NONE',  ( 0.6368676505102698338, 0.000000000000000000, 0.7709731485165541853 ) ) ;
#12158 = CARTESIAN_POINT ( 'NONE',  ( 67.55708173931988370, 20.08915143256180968, 252.2208631684339935 ) ) ;
#12159 = CONTEXT_DEPENDENT_SHAPE_REPRESENTATION ( #1406, #10432 ) ;
#12160 = CARTESIAN_POINT ( 'NONE',  ( -239.0936989914653452, -1.342465038504252250, -11.92464663098946787 ) ) ;
#12161 = DIRECTION ( 'NONE',  ( 0.000000000000000000, 0.000000000000000000, 1.000000000000000000 ) ) ;
#12162 = CARTESIAN_POINT ( 'NONE',  ( -246.7156022632958354, 9.478660875630390947, 6.943882024157772115 ) ) ;
#12163 = ADVANCED_FACE ( 'NONE', ( #9075 ), #855, .F. ) ;
#12164 = ORIENTED_EDGE ( 'NONE', *, *, #1805, .F. ) ;
#12165 = CARTESIAN_POINT ( 'NONE',  ( -239.1649934585021526, -1.429824766643149392, 11.66268491156429299 ) ) ;
#12166 = EDGE_LOOP ( 'NONE', ( #4358, #1136, #10672, #5961 ) ) ;
#12167 = CARTESIAN_POINT ( 'NONE',  ( -238.9324305446047561, 1.023275410052343792, 11.70536273167116015 ) ) ;
#12168 = ORIENTED_EDGE ( 'NONE', *, *, #7960, .F. ) ;
#12169 = UNCERTAINTY_MEASURE_WITH_UNIT (LENGTH_MEASURE( 1.000000000000000082E-05 ), #313, 'distance_accuracy_value', 'NONE');
#12170 = DIRECTION ( 'NONE',  ( 0.5469441386039890496, 0.000000000000000000, -0.8371691043312220470 ) ) ;
#12171 = DIRECTION ( 'NONE',  ( -0.000000000000000000, -1.000000000000000000, 0.000000000000000000 ) ) ;
#12172 = CARTESIAN_POINT ( 'NONE',  ( 0.000000000000000000, 0.000000000000000000, 0.000000000000000000 ) ) ;
#12173 = DIRECTION ( 'NONE',  ( 0.000000000000000000, 0.000000000000000000, -1.000000000000000000 ) ) ;
#12174 = CARTESIAN_POINT ( 'NONE',  ( -190.2689011420770271, 20.08915143297736705, -178.2104428091929549 ) ) ;
#12175 = DIRECTION ( 'NONE',  ( -0.7709731485165534082, 0.000000000000000000, 0.6368676505102708330 ) ) ;
#12176 = EDGE_CURVE ( 'NONE', #3319, #5611, #11073, .T. ) ;
#12177 = EDGE_CURVE ( 'NONE', #3851, #5207, #11139, .T. ) ;
#12178 = CARTESIAN_POINT ( 'NONE',  ( -239.4371284606225743, 1.766671758494314570, -11.86923926621154912 ) ) ;
#12179 = ITEM_DEFINED_TRANSFORMATION ( 'NONE', 'NONE', #6777,  #805 ) ;
#12180 = ORIENTED_EDGE ( 'NONE', *, *, #12657, .T. ) ;
#12181 = CARTESIAN_POINT ( 'NONE',  ( 159.9811538081799540, 20.00000000000000000, 193.6684549073582673 ) ) ;
#12182 = AXIS2_PLACEMENT_3D ( 'NONE', #10300, #6179, #4171 ) ;
#12183 = EDGE_LOOP ( 'NONE', ( #12982, #7108 ) ) ;
#12184 = VECTOR ( 'NONE', #9409, 1000.000000000000000 ) ;
#12185 = CARTESIAN_POINT ( 'NONE',  ( -249.6805863676831336, 11.19144320009710469, -3.579693127732738400 ) ) ;
#12186 = CARTESIAN_POINT ( 'NONE',  ( -247.0556047486957141, -9.588534006571833856, -7.215007616948605040 ) ) ;
#12187 = EDGE_CURVE ( 'NONE', #3500, #552, #10421, .T. ) ;
#12188 = CARTESIAN_POINT ( 'NONE',  ( 34.02434144668578853, 20.08915143297736350, -258.4638482596385529 ) ) ;
#12189 = ORIENTED_EDGE ( 'NONE', *, *, #4259, .T. ) ;
#12190 = AXIS2_PLACEMENT_3D ( 'NONE', #142, #4192, #7333 ) ;
#12191 = CARTESIAN_POINT ( 'NONE',  ( 17.06760680892275062, 20.79694577654979071, 260.7745447056980197 ) ) ;
#12192 = CARTESIAN_POINT ( 'NONE',  ( -246.3021867260495412, 9.336273485133032679, -7.538834026437402080 ) ) ;
#12193 = DIRECTION ( 'NONE',  ( 0.000000000000000000, 1.000000000000000000, 0.000000000000000000 ) ) ;
#12194 = AXIS2_PLACEMENT_3D ( 'NONE', #1961, #4956, #2027 ) ;
#12195 = CARTESIAN_POINT ( 'NONE',  ( -247.4267604613398532, -9.686619269140154032, -6.650504617316419953 ) ) ;
#12196 = AXIS2_PLACEMENT_3D ( 'NONE', #9748, #3623, #7890 ) ;
#12197 = CARTESIAN_POINT ( 'NONE',  ( -249.7379166007384299, 10.64944549068976443, 5.654815128254504053 ) ) ;
#12198 = ADVANCED_FACE ( 'NONE', ( #7012 ), #3997, .F. ) ;
#12199 = CARTESIAN_POINT ( 'NONE',  ( 157.1762463448213225, -19.40000000000000213, 249.7084930171495500 ) ) ;
#12200 = B_SPLINE_CURVE_WITH_KNOTS ( 'NONE', 3,
 ( #3011, #11155, #10089, #962, #1894, #9406, #12407, #6279, #2264, #12089, #11021, #207, #10331, #5966, #4953, #8027, #2946, #3258, #7028, #273, #4330, #8409, #7338, #12470, #5019, #7963, #12030, #3193, #11090, #1957, #6032, #1207, #9091, #5266, #9869, #8738, #9722, #12255, #2718, #6809, #4658, #674, #746, #11814, #8942, #5808, #804, #7735, #7122, #8868, #4046, #5875, #4794, #12868, #4866, #3732, #11870, #2047, #13002, #11936, #3798, #7798, #10867, #9930, #12931, #1740, #1812, #7865, #2787, #8125, #12185, #2657, #6684, #11180, #5670, #9795, #3039, #6116, #10170, #8804, #1049, #6873, #4114, #12798, #10935, #5107, #9185, #61, #8194, #10737, #1608, #3664, #608, #6748, #10799, #1668, #5738, #4727, #5313 ),
 .UNSPECIFIED., .F., .F.,
 ( 4, 2, 2, 1, 1, 2, 2, 2, 2, 1, 1, 1, 2, 2, 2, 2, 1, 1, 1, 1, 2, 2, 2, 2, 1, 1, 1, 1, 2, 2, 2, 2, 2, 2, 1, 1, 1, 1, 2, 2, 2, 2, 1, 1, 1, 1, 2, 2, 2, 2, 1, 1, 1, 1, 2, 2, 2, 2, 1, 1, 2, 2, 4 ),
 ( 0.000000000000000000, 0.03124999999991832922, 0.04687499999987972815, 0.05468749999986047272, 0.05859374999984917620, 0.06054687499984517940, 0.06249999999984116872, 0.09374999999978388121, 0.1093749999997537803, 0.1171874999997375294, 0.1210937499997304517, 0.1230468749997259831, 0.1240234374997236794, 0.1249999999997213895, 0.1874999999997175870, 0.2187499999997155886, 0.2343749999997146727, 0.2421874999997142286, 0.2460937499997137290, 0.2480468749997132016, 0.2490234374997132294, 0.2499999999997132294, 0.3124999999997412070, 0.3437499999997550848, 0.3593749999997621347, 0.3671874999997655764, 0.3710937499997672973, 0.3730468749997681299, 0.3740234374997685185, 0.3749999999997689071, 0.4374999999997900013, 0.4999999999998111511, 0.5624999999998323563, 0.5937499999998429034, 0.6093749999998482325, 0.6171874999998508970, 0.6210937499998521183, 0.6230468749998526734, 0.6240234374998528954, 0.6249999999998531175, 0.6874999999998686606, 0.7187499999998766542, 0.7343749999998807620, 0.7421874999998827604, 0.7460937499998835376, 0.7480468749998843148, 0.7490234374998846478, 0.7499999999998849809, 0.8124999999999326095, 0.8437499999999562572, 0.8593749999999672484, 0.8671874999999736877, 0.8710937499999769074, 0.8730468749999797939, 0.8740234374999813483, 0.8749999999999829026, 0.9062499999999995559, 0.9218750000000092149, 0.9296875000000139888, 0.9335937500000182077, 0.9355468750000203171, 0.9375000000000224265, 1.000000000000000000 ),
 .UNSPECIFIED. ) ;
#12201 = CARTESIAN_POINT ( 'NONE',  ( 17.68709912901472592, -138.4705547276867321, 37.93010648591192080 ) ) ;
#12202 = DIRECTION ( 'NONE',  ( 0.000000000000000000, 0.000000000000000000, 1.000000000000000000 ) ) ;
#12203 = PRODUCT_DEFINITION_SHAPE ( 'NONE', 'NONE',  #13123 ) ;
#12204 = CIRCLE ( 'NONE', #11995, 248.1666666666679930 ) ;
#12205 = B_SPLINE_CURVE_WITH_KNOTS ( 'NONE', 3,
 ( #3958, #2883, #13026, #4154, #7031, #5970, #9228, #8236, #6036, #11093, #5021, #9094, #12291, #10091, #832, #3144, #8030, #4021, #12160, #11292, #7096, #11159, #6098, #10149, #1024, #9158, #2156, #10026, #6965, #5083, #4088, #6233, #3892, #8168, #2086, #12229, #7966, #4892, #3083 ),
 .UNSPECIFIED., .F., .F.,
 ( 4, 2, 2, 2, 1, 1, 2, 2, 2, 1, 1, 2, 2, 2, 2, 1, 1, 1, 2, 2, 2, 2, 4 ),
 ( 0.5002288805836853092, 0.5627002705110166758, 0.6251716604383480425, 0.6329805841792639498, 0.6407895079201798572, 0.6564073554020164458, 0.6876430503656948412, 0.7501144402930455257, 0.7540189021635022026, 0.7579233640339586575, 0.7657322877748720114, 0.7813501352567079339, 0.8125858302203701200, 0.8750572201477042622, 0.8760333356153189310, 0.8770094510829338219, 0.8789616820181391788, 0.8828661438885272439, 0.8906750676292846114, 0.9062929151108138903, 0.9219107625923431693, 0.9375286100738724482, 1.000000000000000000 ),
 .UNSPECIFIED. ) ;
#12206 = CARTESIAN_POINT ( 'NONE',  ( -229.6996680450366171, 1.438960022146944131E-15, 11.75000000000000000 ) ) ;
#12207 = PRESENTATION_LAYER_ASSIGNMENT (  '', '', ( #3677 ) ) ;
#12208 = VERTEX_POINT ( 'NONE', #8692 ) ;
#12209 = ORIENTED_EDGE ( 'NONE', *, *, #9422, .T. ) ;
#12210 = CARTESIAN_POINT ( 'NONE',  ( -17.05314194221659818, 20.08915143297737416, -260.5542428351129729 ) ) ;
#12211 = FACE_OUTER_BOUND ( 'NONE', #1688, .T. ) ;
#12212 = CYLINDRICAL_SURFACE ( 'NONE', #430, 5.500000000000005329 ) ;
#12213 = CIRCLE ( 'NONE', #2413, 6.500000000000005329 ) ;
#12214 = DIRECTION ( 'NONE',  ( 0.000000000000000000, 1.000000000000000000, 0.000000000000000000 ) ) ;
#12215 = CONICAL_SURFACE ( 'NONE', #1132, 3.000000000000000000, 0.7853981633974461696 ) ;
#12216 = CARTESIAN_POINT ( 'NONE',  ( -185.9653539489998195, -30.00000000000000000, -225.1241593668329699 ) ) ;
#12217 = CARTESIAN_POINT ( 'NONE',  ( -10.83189848055848969, -138.4705547276867321, 40.42519547187230700 ) ) ;
#12218 = AXIS2_PLACEMENT_3D ( 'NONE', #5751, #11881, #11757 ) ;
#12219 = CARTESIAN_POINT ( 'NONE',  ( -243.2974363556361084, -7.571041504521477172, 8.986772704220435060 ) ) ;
#12220 = VERTEX_POINT ( 'NONE', #947 ) ;
#12221 = DIRECTION ( 'NONE',  ( 8.659560562354939021E-17, 0.7071067811865470176, -0.7071067811865480168 ) ) ;
#12222 = CARTESIAN_POINT ( 'NONE',  ( 0.000000000000000000, 23.50000000000000000, 0.000000000000000000 ) ) ;
#12223 = ORIENTED_EDGE ( 'NONE', *, *, #2684, .T. ) ;
#12224 = ORIENTED_EDGE ( 'NONE', *, *, #8271, .F. ) ;
#12225 = AXIS2_PLACEMENT_3D ( 'NONE', #6837, #10898, #8899 ) ;
#12226 = CARTESIAN_POINT ( 'NONE',  ( -122.2593324768359935, 30.00000000000000000, -168.2755348299880040 ) ) ;
#12227 = DIRECTION ( 'NONE',  ( 0.000000000000000000, 0.000000000000000000, -1.000000000000000000 ) ) ;
#12228 = CARTESIAN_POINT ( 'NONE',  ( 252.2208631679629889, 20.08915143265645042, -67.55708173926119287 ) ) ;
#12229 = CARTESIAN_POINT ( 'NONE',  ( -239.6598046804633384, -1.963348619657336425, -11.83831708221096690 ) ) ;
#12230 = DIRECTION ( 'NONE',  ( -0.3420201433256694346, 0.000000000000000000, 0.9396926207859080948 ) ) ;
#12231 = CARTESIAN_POINT ( 'NONE',  ( -242.2247058965207316, 6.524571383469930375, 9.772025480168560208 ) ) ;
#12232 = EDGE_CURVE ( 'NONE', #8469, #5922, #1061, .T. ) ;
#12233 = EDGE_CURVE ( 'NONE', #9495, #3412, #8368, .T. ) ;
#12234 = PRODUCT_DEFINITION_SHAPE ( 'NONE', 'NONE',  #13090 ) ;
#12235 = AXIS2_PLACEMENT_3D ( 'NONE', #11174, #5100, #6181 ) ;
#12237 = EDGE_LOOP ( 'NONE', ( #5058, #2409, #4042, #10901, #12224 ) ) ;
#12236 = AXIS2_PLACEMENT_3D ( 'NONE', #11998, #8132, #2979 ) ;
#12238 = CARTESIAN_POINT ( 'NONE',  ( 229.2637990951503753, -30.00000000000000000, -180.9540284836414514 ) ) ;
#12239 = VERTEX_POINT ( 'NONE', #1627 ) ;
#12240 = DIRECTION ( 'NONE',  ( -0.000000000000000000, -1.000000000000000000, 0.000000000000000000 ) ) ;
#12241 = EDGE_LOOP ( 'NONE', ( #6089, #3857 ) ) ;
#12242 = VECTOR ( 'NONE', #4912, 1000.000000000000000 ) ;
#12243 = CARTESIAN_POINT ( 'NONE',  ( 135.8846079354933352, -30.00000000000000000, -256.1940150085812888 ) ) ;
#12244 = DIRECTION ( 'NONE',  ( 0.000000000000000000, -1.000000000000000000, 0.000000000000000000 ) ) ;
#12245 = FACE_OUTER_BOUND ( 'NONE', #8885, .T. ) ;
#12246 = CARTESIAN_POINT ( 'NONE',  ( -171.8850263962752649, 20.08915143297736350, -196.0019244007921486 ) ) ;
#12247 = CARTESIAN_POINT ( 'NONE',  ( -210.0000000000000000, 19.40000000000000213, -5.100000000000000533 ) ) ;
#12248 = CARTESIAN_POINT ( 'NONE',  ( 122.2593324768334071, 29.00000000000000000, -173.7755348299895104 ) ) ;
#12249 = CONTEXT_DEPENDENT_SHAPE_REPRESENTATION ( #6429, #2451 ) ;
#12250 = ORIENTED_EDGE ( 'NONE', *, *, #9658, .T. ) ;
#12251 = PLANE ( 'NONE',  #8385 ) ;
#12252 = AXIS2_PLACEMENT_3D ( 'NONE', #392, #1521, #526 ) ;
#12253 = ORIENTED_EDGE ( 'NONE', *, *, #9805, .T. ) ;
#12254 = CIRCLE ( 'NONE', #10330, 230.0000000000000000 ) ;
#12255 = CARTESIAN_POINT ( 'NONE',  ( -249.7621493471160363, 11.48044694377630925, 2.508021713178596013 ) ) ;
#12256 = CARTESIAN_POINT ( 'NONE',  ( -244.8027971735998847, -8.628165349708508458, -8.339952776884981489 ) ) ;
#12257 = CARTESIAN_POINT ( 'NONE',  ( -249.6784491604580296, -11.18557168011258618, 3.597985675147115980 ) ) ;
#12258 = VERTEX_POINT ( 'NONE', #12142 ) ;
#12259 = EDGE_CURVE ( 'NONE', #11682, #8685, #6770, .T. ) ;
#12260 = CARTESIAN_POINT ( 'NONE',  ( -260.7745447056980197, 20.79694577654979071, 17.06760680913495065 ) ) ;
#12261 = EDGE_CURVE ( 'NONE', #11582, #9692, #4685, .T. ) ;
#12262 = CARTESIAN_POINT ( 'NONE',  ( -247.9529057710629445, 9.807895050960942385, -6.914131050859374739 ) ) ;
#12263 = DIRECTION ( 'NONE',  ( 0.000000000000000000, 1.000000000000000000, 0.000000000000000000 ) ) ;
#12264 = CARTESIAN_POINT ( 'NONE',  ( -245.5121636064574773, -8.994012747014300757, -7.561165846882150987 ) ) ;
#12265 =( REPRESENTATION_RELATIONSHIP ('NONE','NONE', #12019, #5191 ) REPRESENTATION_RELATIONSHIP_WITH_TRANSFORMATION ( #11664 )SHAPE_REPRESENTATION_RELATIONSHIP( ) );
#12266 = CARTESIAN_POINT ( 'NONE',  ( -0.000000000000000000, -18.00000000000000000, 0.000000000000000000 ) ) ;
#12267 = CARTESIAN_POINT ( 'NONE',  ( 41.21542755584187034, -138.4705547276867321, 7.267391899530501576 ) ) ;
#12268 = DIRECTION ( 'NONE',  ( -0.000000000000000000, -1.000000000000000000, 0.000000000000000000 ) ) ;
#12269 = CARTESIAN_POINT ( 'NONE',  ( 227.3999999999999773, -0.1281080013181084831, -6.498737441995811714 ) ) ;
#12270 = VERTEX_POINT ( 'NONE', #274 ) ;
#12271 = EDGE_LOOP ( 'NONE', ( #5278, #10833, #4625, #5242 ) ) ;
#12272 = CARTESIAN_POINT ( 'NONE',  ( -252.2208631662124958, 20.08915143301432948, -67.55708173888800161 ) ) ;
#12273 = EDGE_CURVE ( 'NONE', #5446, #2165, #636, .T. ) ;
#12274 = LINE ( 'NONE', #8146, #4167 ) ;
#12275 = CARTESIAN_POINT ( 'NONE',  ( 239.1910253111499287, -1.013189013416512463, -3.350157823600272700 ) ) ;
#12276 = DIRECTION ( 'NONE',  ( 0.000000000000000000, 0.9998057603070481525, -0.01970892327970899874 ) ) ;
#12277 = CARTESIAN_POINT ( 'NONE',  ( 207.3438552925264844, 20.79694577678052880, -159.0697709836649949 ) ) ;
#12278 = EDGE_CURVE ( 'NONE', #11418, #6295, #5744, .T. ) ;
#12279 = CARTESIAN_POINT ( 'NONE',  ( 165.7021400752470868, -1.848645179577134812, 200.5941117395223046 ) ) ;
#12280 = DIRECTION ( 'NONE',  ( 0.8660254037844328234, 0.000000000000000000, 0.5000000000000101030 ) ) ;
#12281 = DIRECTION ( 'NONE',  ( 0.6368676505102696117, 0.000000000000000000, 0.7709731485165545184 ) ) ;
#12282 = ORIENTED_EDGE ( 'NONE', *, *, #9431, .F. ) ;
#12283 = DIRECTION ( 'NONE',  ( -0.6368676505102707219, 0.000000000000000000, -0.7709731485165535192 ) ) ;
#12284 = CARTESIAN_POINT ( 'NONE',  ( 27.68945685411497593, -19.00000000000000000, -290.6841825403026291 ) ) ;
#12285 = ORIENTED_EDGE ( 'NONE', *, *, #579, .T. ) ;
#12286 = VERTEX_POINT ( 'NONE', #11409 ) ;
#12287 = DIRECTION ( 'NONE',  ( 1.000000000000000000, 0.000000000000000000, 0.000000000000000000 ) ) ;
#12288 = DIRECTION ( 'NONE',  ( 0.6368676505102707219, 0.000000000000000000, 0.7709731485165535192 ) ) ;
#12289 = CARTESIAN_POINT ( 'NONE',  ( 34.10614053541959834, 20.08915143339292442, 258.8746690701424882 ) ) ;
#12290 = AXIS2_PLACEMENT_3D ( 'NONE', #5308, #2651, #4853 ) ;
#12291 = CARTESIAN_POINT ( 'NONE',  ( -238.9758744801582395, -1.144350540312424558, -11.94573993414358704 ) ) ;
#12292 = CARTESIAN_POINT ( 'NONE',  ( 0.000000000000000000, -138.4705547276867321, 41.85124196045095601 ) ) ;
#12293 = CARTESIAN_POINT ( 'NONE',  ( -246.4924783649346125, 9.403937930409544066, 7.045599365780679690 ) ) ;
#12294 = ORIENTED_EDGE ( 'NONE', *, *, #6723, .T. ) ;
#12295 = CARTESIAN_POINT ( 'NONE',  ( 130.4544329367266471, 20.79694577634646180, 225.9597979674046542 ) ) ;
#12296 = ORIENTED_EDGE ( 'NONE', *, *, #3748, .F. ) ;
#12297 = DIRECTION ( 'NONE',  ( 0.6368676505102716101, 0.000000000000000000, 0.7709731485165527420 ) ) ;
#12298 = ORIENTED_EDGE ( 'NONE', *, *, #12397, .F. ) ;
#12299 = ORIENTED_EDGE ( 'NONE', *, *, #2286, .F. ) ;
#12300 = CIRCLE ( 'NONE', #6769, 240.3921568627444856 ) ;
#12301 = APPLICATION_CONTEXT ( 'automotive_design' ) ;
#12302 = EDGE_CURVE ( 'NONE', #4412, #1244, #7341, .T. ) ;
#12303 = DIRECTION ( 'NONE',  ( 0.6368676505102737195, 0.000000000000000000, 0.7709731485165509657 ) ) ;
#12304 = LINE ( 'NONE', #6313, #1266 ) ;
#12305 = CARTESIAN_POINT ( 'NONE',  ( 239.0740262672538563, 0.7008254641484221725, 3.430151065625266060 ) ) ;
#12306 = CARTESIAN_POINT ( 'NONE',  ( 185.9653539490014111, -30.00000000000000000, 225.1241593668316625 ) ) ;
#12307 = CARTESIAN_POINT ( 'NONE',  ( -17.05322212017792793, 20.08915143297736705, -260.1353576186481860 ) ) ;
#12308 = DIRECTION ( 'NONE',  ( 0.000000000000000000, 0.000000000000000000, 1.000000000000000000 ) ) ;
#12309 = AXIS2_PLACEMENT_3D ( 'NONE', #9293, #4217, #9159 ) ;
#12310 = ORIENTED_EDGE ( 'NONE', *, *, #2638, .F. ) ;
#12311 = CARTESIAN_POINT ( 'NONE',  ( 0.000000000000000000, -13.19999999999999929, 0.000000000000000000 ) ) ;
#12312 = ORIENTED_EDGE ( 'NONE', *, *, #12017, .T. ) ;
#12313 = CARTESIAN_POINT ( 'NONE',  ( 122.2593324768334071, 30.00000000000000000, -162.7755348299894820 ) ) ;
#12314 = CARTESIAN_POINT ( 'NONE',  ( -245.7174131604188858, -9.095590352148393620, -7.828444976190365168 ) ) ;
#12315 =( REPRESENTATION_RELATIONSHIP ('NONE','NONE', #12019, #182 ) REPRESENTATION_RELATIONSHIP_WITH_TRANSFORMATION ( #3561 )SHAPE_REPRESENTATION_RELATIONSHIP( ) );
#12316 = CARTESIAN_POINT ( 'NONE',  ( -249.7845350862966995, -11.60862138559210877, 1.817256862172399234 ) ) ;
#12317 = CIRCLE ( 'NONE', #5288, 249.2999999999999829 ) ;
#12318 = EDGE_LOOP ( 'NONE', ( #765, #310, #1490, #11303 ) ) ;
#12319 = CIRCLE ( 'NONE', #6367, 304.0000000000000000 ) ;
#12320 = TOROIDAL_SURFACE ( 'NONE', #5000, 2.750000000000000000, 0.8000000000000000444 ) ;
#12321 = EDGE_CURVE ( 'NONE', #6953, #8515, #11917, .T. ) ;
#12322 = CIRCLE ( 'NONE', #398, 239.8169934640564804 ) ;
#12323 = AXIS2_PLACEMENT_3D ( 'NONE', #6216, #8223, #9143 ) ;
#12324 = CARTESIAN_POINT ( 'NONE',  ( -172.3268284098719789, 20.79694577634883856, 196.4640694352564765 ) ) ;
#12325 = CARTESIAN_POINT ( 'NONE',  ( -244.1419029264685605, 8.215433989563221573, -8.746719778180930049 ) ) ;
#12326 = DIRECTION ( 'NONE',  ( 0.000000000000000000, 0.000000000000000000, -1.000000000000000000 ) ) ;
#12327 = APPLICATION_CONTEXT ( 'automotive_design' ) ;
#12328 = AXIS2_PLACEMENT_3D ( 'NONE', #6506, #12562, #10563 ) ;
#12329 = CARTESIAN_POINT ( 'NONE',  ( -242.3794917446704460, -6.695067658966850743, -9.656064786588574478 ) ) ;
#12330 = CARTESIAN_POINT ( 'NONE',  ( 239.2930894855859947, -1.216635601170958036, 3.281912597181230407 ) ) ;
#12331 = DIRECTION ( 'NONE',  ( 0.6820219226572394877, 0.5538822189107470706, 0.4775568914688905209 ) ) ;
#12332 = ADVANCED_FACE ( 'NONE', ( #82 ), #5093, .F. ) ;
#12333 = CARTESIAN_POINT ( 'NONE',  ( 0.000000000000000000, 19.00000000000000000, -202.4999999999999716 ) ) ;
#12334 = ITEM_DEFINED_TRANSFORMATION ( 'NONE', 'NONE', #9790,  #805 ) ;
#12335 = EDGE_CURVE ( 'NONE', #12702, #9039, #1141, .T. ) ;
#12336 = AXIS2_PLACEMENT_3D ( 'NONE', #5208, #5345, #12351 ) ;
#12337 = CARTESIAN_POINT ( 'NONE',  ( 0.000000000000000000, -2.957522019940860139E-14, 0.000000000000000000 ) ) ;
#12338 = ORIENTED_EDGE ( 'NONE', *, *, #2415, .T. ) ;
#12339 = CARTESIAN_POINT ( 'NONE',  ( -83.95474316008289861, 20.08915143298712280, -247.2466869553079789 ) ) ;
#12340 = DIRECTION ( 'NONE',  ( 0.000000000000000000, -0.7071067811865489050, -0.7071067811865460184 ) ) ;
#12341 = CARTESIAN_POINT ( 'NONE',  ( 208.1627500994694628, 20.00000000000000000, -171.9542656377731191 ) ) ;
#12342 = DIRECTION ( 'NONE',  ( 0.6368676505102708330, 0.000000000000000000, 0.7709731485165535192 ) ) ;
#12343 = CARTESIAN_POINT ( 'NONE',  ( -248.9599100169513122, -9.954851740894934409, 6.700860962374001417 ) ) ;
#12344 = DIRECTION ( 'NONE',  ( 0.000000000000000000, 1.000000000000000000, 0.000000000000000000 ) ) ;
#12345 = DIRECTION ( 'NONE',  ( 0.9396926207859128688, 0.000000000000000000, -0.3420201433256569445 ) ) ;
#12346 = EDGE_CURVE ( 'NONE', #204, #4826, #7448, .T. ) ;
#12347 = CARTESIAN_POINT ( 'NONE',  ( 27.68945685411497593, -30.00000000000000000, -290.6841825403026291 ) ) ;
#12348 = CONTEXT_DEPENDENT_SHAPE_REPRESENTATION ( #9084, #6030 ) ;
#12349 = ADVANCED_FACE ( 'NONE', ( #6281, #1208 ), #1005, .F. ) ;
#12350 = ORIENTED_EDGE ( 'NONE', *, *, #8077, .T. ) ;
#12351 = DIRECTION ( 'NONE',  ( 0.000000000000000000, 0.000000000000000000, 1.000000000000000000 ) ) ;
#12352 = CIRCLE ( 'NONE', #10642, 6.499999999999999112 ) ;
#12353 = PRODUCT_DEFINITION_SHAPE ( 'NONE', 'NONE',  #13042 ) ;
#12354 = CARTESIAN_POINT ( 'NONE',  ( 229.9849328834052926, -2.312147543537095729, -2.637679212737643386 ) ) ;
#12355 = ORIENTED_EDGE ( 'NONE', *, *, #252, .T. ) ;
#12356 = ORIENTED_EDGE ( 'NONE', *, *, #2529, .T. ) ;
#12357 = EDGE_CURVE ( 'NONE', #7179, #5643, #12409, .T. ) ;
#12358 = CARTESIAN_POINT ( 'NONE',  ( 235.4000000000000057, 0.000000000000000000, 0.000000000000000000 ) ) ;
#12359 = LINE ( 'NONE', #2083, #3148 ) ;
#12360 = CARTESIAN_POINT ( 'NONE',  ( 34.18476129304277578, 19.96883745937039834, 259.4723857425807978 ) ) ;
#12361 = DIRECTION ( 'NONE',  ( -0.6368676505102707219, 0.000000000000000000, -0.7709731485165536302 ) ) ;
#12362 = DIRECTION ( 'NONE',  ( 0.000000000000000000, 0.000000000000000000, 1.000000000000000000 ) ) ;
#12363 = CARTESIAN_POINT ( 'NONE',  ( -244.5179878702206793, 8.451416885157774672, 8.163389686018202696 ) ) ;
#12364 = AXIS2_PLACEMENT_3D ( 'NONE', #601, #2852, #1664 ) ;
#12365 = ADVANCED_FACE ( 'NONE', ( #8147 ), #12212, .F. ) ;
#12366 = VERTEX_POINT ( 'NONE', #11204 ) ;
#12367 = CARTESIAN_POINT ( 'NONE',  ( -165.7021400752471436, -1.848645179577134812, -200.5941117395223046 ) ) ;
#12368 = EDGE_LOOP ( 'NONE', ( #2569, #4741, #694, #7740 ) ) ;
#12369 = CARTESIAN_POINT ( 'NONE',  ( 0.000000000000000000, 22.00000000000000000, 0.000000000000000000 ) ) ;
#12370 = ORIENTED_EDGE ( 'NONE', *, *, #1916, .F. ) ;
#12371 = ORIENTED_EDGE ( 'NONE', *, *, #7250, .F. ) ;
#12372 = DIRECTION ( 'NONE',  ( 0.000000000000000000, 0.000000000000000000, 1.000000000000000000 ) ) ;
#12373 = CARTESIAN_POINT ( 'NONE',  ( -239.7835669211240202, 2.057906893573868246, -11.82250766619783278 ) ) ;
#12374 = LINE ( 'NONE', #373, #4456 ) ;
#12375 = LINE ( 'NONE', #5982, #3654 ) ;
#12376 = CARTESIAN_POINT ( 'NONE',  ( -238.7110722354929067, 0.02061376086992028692, -11.74998185356844438 ) ) ;
#12377 = SURFACE_SIDE_STYLE ('',( #8319 ) ) ;
#12378 = CONTEXT_DEPENDENT_SHAPE_REPRESENTATION ( #10003, #12963 ) ;
#12379 = ORIENTED_EDGE ( 'NONE', *, *, #9825, .T. ) ;
#12380 = DIRECTION ( 'NONE',  ( -1.000000000000000000, 0.000000000000000000, 0.000000000000000000 ) ) ;
#12381 = CIRCLE ( 'NONE', #3856, 5.100000000000000533 ) ;
#12382 = CONICAL_SURFACE ( 'NONE', #490, 3.000000000000000000, 0.7853981633974490562 ) ;
#12383 = ORIENTED_EDGE ( 'NONE', *, *, #4271, .F. ) ;
#12384 = DIRECTION ( 'NONE',  ( 0.000000000000000000, 0.9998057603070480415, -0.01970892327970899527 ) ) ;
#12385 = CARTESIAN_POINT ( 'NONE',  ( -242.9129853705333915, -7.240649581379505761, -9.569633194163635892 ) ) ;
#12386 = CARTESIAN_POINT ( 'NONE',  ( -249.2901971947345032, -10.52637179445247284, 5.220957665109235535 ) ) ;
#12387 = ORIENTED_EDGE ( 'NONE', *, *, #5038, .T. ) ;
#12388 = CARTESIAN_POINT ( 'NONE',  ( -17.06760680892479698, 20.79694577614318973, 260.7745447066434963 ) ) ;
#12389 = CARTESIAN_POINT ( 'NONE',  ( -241.1422742070761558, 5.089614320685067916, -10.87069852639233147 ) ) ;
#12390 = CARTESIAN_POINT ( 'NONE',  ( 235.4000000000000057, -0.1024105694488001289, -5.195143123655522110 ) ) ;
#12391 = CARTESIAN_POINT ( 'NONE',  ( -241.4660365540256635, -5.559932090034945595, -10.35152193387608044 ) ) ;
#12392 = CIRCLE ( 'NONE', #8144, 6.500000000000005329 ) ;
#12393 = CARTESIAN_POINT ( 'NONE',  ( 238.9937480945849018, -0.3586231069789287407, 3.486222115773272900 ) ) ;
#12394 = APPLICATION_PROTOCOL_DEFINITION ( 'draft international standard', 'automotive_design', 1998, #6854 ) ;
#12395 = EDGE_CURVE ( 'NONE', #1017, #7886, #5267, .T. ) ;
#12396 = DIRECTION ( 'NONE',  ( 0.000000000000000000, -0.01970892327970900221, -0.9998057603070482635 ) ) ;
#12397 = EDGE_CURVE ( 'NONE', #4274, #9366, #2068, .T. ) ;
#12398 = AXIS2_PLACEMENT_3D ( 'NONE', #8615, #9598, #6420 ) ;
#12399 =( REPRESENTATION_RELATIONSHIP ('NONE','NONE', #12019, #182 ) REPRESENTATION_RELATIONSHIP_WITH_TRANSFORMATION ( #883 )SHAPE_REPRESENTATION_RELATIONSHIP( ) );
#12400 = CARTESIAN_POINT ( 'NONE',  ( 0.000000000000000000, 29.00000000000000000, -249.7999999999999829 ) ) ;
#12401 = VERTEX_POINT ( 'NONE', #1070 ) ;
#12402 = B_SPLINE_CURVE_WITH_KNOTS ( 'NONE', 3,
 ( #7661, #4588, #2849, #8733, #3593, #4719, #4855, #5870 ),
 .UNSPECIFIED., .F., .F.,
 ( 4, 2, 2, 4 ),
 ( 0.000000000000000000, 0.2500000000000098255, 0.5000000000000196509, 1.000000000000000000 ),
 .UNSPECIFIED. ) ;
#12403 = CONICAL_SURFACE ( 'NONE', #13035, 5.499999999999986677, 0.7853981633974461696 ) ;
#12404 = CARTESIAN_POINT ( 'NONE',  ( 83.95474316006190918, 20.08915143290042948, -247.2466869557860036 ) ) ;
#12405 = CARTESIAN_POINT ( 'NONE',  ( -138.9238112054132444, -23.50000000000000000, 212.6409525001303678 ) ) ;
#12406 = CIRCLE ( 'NONE', #12196, 5.500000000000005329 ) ;
#12407 = CARTESIAN_POINT ( 'NONE',  ( -248.7201528608048307, 10.06060527423840334, 6.070293049067540636 ) ) ;
#12408 = EDGE_CURVE ( 'NONE', #6668, #3483, #5628, .T. ) ;
#12409 = LINE ( 'NONE', #4070, #8312 ) ;
#12410 = DIRECTION ( 'NONE',  ( 0.000000000000000000, 0.000000000000000000, 1.000000000000000000 ) ) ;
#12411 = DIRECTION ( 'NONE',  ( 1.000000000000000000, 0.000000000000000000, 0.000000000000000000 ) ) ;
#12412 = DIRECTION ( 'NONE',  ( 0.000000000000000000, 1.000000000000000000, 0.000000000000000000 ) ) ;
#12413 = DIRECTION ( 'NONE',  ( -0.1445786100688102871, 0.5538822189107471816, 0.8199460427888399794 ) ) ;
#12414 = VECTOR ( 'NONE', #6414, 1000.000000000000227 ) ;
#12415 = CARTESIAN_POINT ( 'NONE',  ( 71.82423009839129691, 19.40000000000000213, -192.2354503650404922 ) ) ;
#12416 = VERTEX_POINT ( 'NONE', #9526 ) ;
#12417 = DIRECTION ( 'NONE',  ( 0.6368676505102707219, 0.000000000000000000, 0.7709731485165535192 ) ) ;
#12418 = DIRECTION ( 'NONE',  ( -0.6368676505102696117, 0.000000000000000000, -0.7709731485165545184 ) ) ;
#12419 = VERTEX_POINT ( 'NONE', #12721 ) ;
#12420 = ORIENTED_EDGE ( 'NONE', *, *, #10363, .F. ) ;
#12421 = CARTESIAN_POINT ( 'NONE',  ( 71.82423009839129691, 19.40000000000000213, 197.3354503650404865 ) ) ;
#12422 = EDGE_CURVE ( 'NONE', #10097, #4274, #2120, .T. ) ;
#12423 = CIRCLE ( 'NONE', #5396, 6.500000000000005329 ) ;
#12424 = CIRCLE ( 'NONE', #12844, 230.0000000000000000 ) ;
#12425 = EDGE_CURVE ( 'NONE', #12854, #4597, #3526, .T. ) ;
#12426 = CONICAL_SURFACE ( 'NONE', #10509, 6.500000000000005329, 0.7853981633974490562 ) ;
#12427 = CARTESIAN_POINT ( 'NONE',  ( -67.76049180241520276, 20.55460285097757378, 252.9796497716870078 ) ) ;
#12428 = CARTESIAN_POINT ( 'NONE',  ( 194.2446334056324986, -29.00000000000000000, 235.1468102975487966 ) ) ;
#12429 = CARTESIAN_POINT ( 'NONE',  ( 0.000000000000000000, 0.000000000000000000, 0.000000000000000000 ) ) ;
#12430 = CARTESIAN_POINT ( 'NONE',  ( -240.6673884781993706, 4.184756593251726997, 10.97954905608461118 ) ) ;
#12431 = ORIENTED_EDGE ( 'NONE', *, *, #6630, .F. ) ;
#12432 = CARTESIAN_POINT ( 'NONE',  ( 244.1900186690936039, 20.79694577634646890, 91.90986972409962164 ) ) ;
#12433 = VERTEX_POINT ( 'NONE', #2399 ) ;
#12434 = DIRECTION ( 'NONE',  ( 8.659560562354913137E-17, -0.7071067811865489050, 0.7071067811865460184 ) ) ;
#12435 = VERTEX_POINT ( 'NONE', #5465 ) ;
#12436 = VERTEX_POINT ( 'NONE', #6675 ) ;
#12437 =( REPRESENTATION_RELATIONSHIP ('NONE','NONE', #12019, #5191 ) REPRESENTATION_RELATIONSHIP_WITH_TRANSFORMATION ( #3777 )SHAPE_REPRESENTATION_RELATIONSHIP( ) );
#12438 = DIRECTION ( 'NONE',  ( 0.000000000000000000, 0.9998057603070480415, -0.01970892327970899874 ) ) ;
#12439 = ADVANCED_FACE ( 'NONE', ( #3458 ), #405, .F. ) ;
#12440 = FACE_BOUND ( 'NONE', #11956, .T. ) ;
#12441 = DIRECTION ( 'NONE',  ( 0.000000000000000000, 0.000000000000000000, -1.000000000000000000 ) ) ;
#12442 = CARTESIAN_POINT ( 'NONE',  ( 239.2087834362114052, 1.051957556968997842, -3.338183402669812505 ) ) ;
#12443 = CIRCLE ( 'NONE', #741, 251.8333333333299606 ) ;
#12444 = CARTESIAN_POINT ( 'NONE',  ( -238.9571511871961320, 1.076409201234731272, -11.70061098712747594 ) ) ;
#12445 = CARTESIAN_POINT ( 'NONE',  ( -245.7174131648644675, 9.095590354146871448, 7.828444973944560736 ) ) ;
#12446 = PLANE ( 'NONE',  #12835 ) ;
#12447 =( BOUNDED_SURFACE ( )  B_SPLINE_SURFACE ( 3, 3, ( 
 ( #4891, #12894, #3891, #1835, #6902, #7762, #2743, #6832, #11894, #4754, #770, #5897, #4817, #10823, #8964, #10893, #5766, #705, #8830, #13025, #11837, #1768, #11708, #8895, #12958, #6641, #10697, #1572, #6708, #12759, #8763, #3824, #1630, #9690, #4616, #8693, #7694, #11773, #2621, #12827, #10090, #1160, #5217, #2949, #9291, #12091, #12228, #6035, #7910, #4152, #7029, #2025, #963, #5020, #9092, #1896, #1022, #6097, #2882, #2788, #7230, #10024, #12158, #12289, #11091, #4020 ),
 ( #8098, #11290, #3956, #11220, #9157, #10284, #6964, #8167, #2152, #3012, #1960, #10148, #3143, #30, #7095, #5082, #9031, #11158, #4087, #3081, #896, #11022, #6232, #7161, #8029, #162, #7965, #2085, #6162, #10217, #1089, #12031, #5147, #5968, #99, #9227, #8235, #4955, #11559, #6299, #5283, #296, #2417, #10417, #3276, #3478, #4352, #10348, #3210, #1484, #7358, #2221, #3338, #12614, #6496, #7417, #8300, #6557, #5356, #423, #5423, #10552, #8363, #12360, #1222, #1421 ),
 ( #2280, #9359, #4472, #12427, #11490, #6360, #1292, #9427, #11360, #10490, #2353, #7293, #8429, #7553, #225, #12484, #8555, #11424, #6426, #12549, #1358, #9487, #4283, #8492, #358, #4406, #3405, #7488, #11624, #5480, #2478, #10614, #9603, #9540, #5547, #4215, #2544, #11822, #10875, #8677, #12739, #5818, #6692, #556, #9879, #3608, #491, #7676, #4601, #11879, #6622, #12808, #1749, #6883, #12939, #3540, #2666, #7612, #4736, #7875, #6755, #756, #4804, #11754, #2605, #617 ),
 ( #10676, #12681, #10946, #10745, #11691, #3674, #8876, #7805, #7747, #4539, #2796, #1616, #5680, #1681, #1817, #9732, #1550, #8815, #4668, #3807, #8747, #5615, #10808, #9673, #5748, #9804, #5885, #11947, #8622, #684, #3741, #12877, #2727, #6819, #6949, #13010, #1943, #3873, #3067, #5132, #9194, #9208, #12277, #11074, #811, #9938, #6145, #10201, #10010, #2069, #5064, #3939, #7147, #2864, #2138, #1007, #1073, #2011, #12073, #12016, #7945, #4285, #8949, #4873, #17, #85 ) ),
 .UNSPECIFIED., .F., .T., .T. ) 
 B_SPLINE_SURFACE_WITH_KNOTS ( ( 4, 4 ),
 ( 4, 2, 2, 2, 2, 2, 2, 2, 2, 2, 2, 2, 2, 2, 2, 2, 2, 2, 2, 2, 2, 2, 2, 2, 2, 2, 2, 2, 2, 2, 2, 2, 4 ),
 ( 0.000000000000000000, 1.000000000000000000 ),
 ( 0.5000000000000000000, 0.5312500000000000000, 0.5625000000000000000, 0.5937500000000000000, 0.6250000000000000000, 0.6562500000000000000, 0.6875000000000000000, 0.7187500000000000000, 0.7500000000000000000, 0.7812500000000000000, 0.8125000000000000000, 0.8437500000000000000, 0.8750000000000000000, 0.9062500000000000000, 0.9375000000000000000, 0.9687500000000000000, 1.000000000000000000, 1.031250000000000000, 1.062500000000000000, 1.093750000000000000, 1.125000000000000000, 1.156250000000000000, 1.187500000000000000, 1.218750000000000000, 1.250000000000000000, 1.281250000000000000, 1.312500000000000000, 1.343750000000000000, 1.375000000000000000, 1.406250000000000000, 1.437500000000000000, 1.468750000000000000, 1.500000000000000000 ),
 .UNSPECIFIED. ) 
 GEOMETRIC_REPRESENTATION_ITEM ( )  RATIONAL_B_SPLINE_SURFACE ( (
 ( 1.000000000000000000, 1.000000000000000000, 1.000000000000000000, 1.000000000000000000, 1.000000000000000000, 1.000000000000000000, 1.000000000000000000, 1.000000000000000000, 1.000000000000000000, 1.000000000000000000, 1.000000000000000000, 1.000000000000000000, 1.000000000000000000, 1.000000000000000000, 1.000000000000000000, 1.000000000000000000, 1.000000000000000000, 1.000000000000000000, 1.000000000000000000, 1.000000000000000000, 1.000000000000000000, 1.000000000000000000, 1.000000000000000000, 1.000000000000000000, 1.000000000000000000, 1.000000000000000000, 1.000000000000000000, 1.000000000000000000, 1.000000000000000000, 1.000000000000000000, 1.000000000000000000, 1.000000000000000000, 1.000000000000000000, 1.000000000000000000, 1.000000000000000000, 1.000000000000000000, 1.000000000000000000, 1.000000000000000000, 1.000000000000000000, 1.000000000000000000, 1.000000000000000000, 1.000000000000000000, 1.000000000000000000, 1.000000000000000000, 1.000000000000000000, 1.000000000000000000, 1.000000000000000000, 1.000000000000000000, 1.000000000000000000, 1.000000000000000000, 1.000000000000000000, 1.000000000000000000, 1.000000000000000000, 1.000000000000000000, 1.000000000000000000, 1.000000000000000000, 1.000000000000000000, 1.000000000000000000, 1.000000000000000000, 1.000000000000000000, 1.000000000000000000, 1.000000000000000000, 1.000000000000000000, 1.000000000000000000, 1.000000000000000000, 1.000000000000000000),
 ( 0.4027746460044325238, 0.4027746460044325238, 0.4027746460044540067, 0.4027746460044540067, 0.4027746460044225318, 0.4027746460044225318, 0.4027746460043825083, 0.4027746460043825083, 0.4027746460043430399, 0.4027746460043430399, 0.4027746460043289956, 0.4027746460043289956, 0.4027746460043410415, 0.4027746460043410415, 0.4027746460044525079, 0.4027746460044525079, 0.4027746460044325238, 0.4027746460044325238, 0.4027746460044525079, 0.4027746460044525079, 0.4027746460043595267, 0.4027746460043595267, 0.4027746460044215326, 0.4027746460044215326, 0.4027746460043590271, 0.4027746460043590271, 0.4027746460044335230, 0.4027746460044335230, 0.4027746460043410415, 0.4027746460043410415, 0.4027746460042145316, 0.4027746460042145316, 0.4027746460044325238, 0.4027746460044325238, 0.4027746460044535071, 0.4027746460044535071, 0.4027746460044230314, 0.4027746460044230314, 0.4027746460043575283, 0.4027746460043575283, 0.4027746460043590271, 0.4027746460043590271, 0.4027746460043944987, 0.4027746460043944987, 0.4027746460043630239, 0.4027746460043630239, 0.4027746460044520083, 0.4027746460044520083, 0.4027746460044325238, 0.4027746460044325238, 0.4027746460044530075, 0.4027746460044530075, 0.4027746460043180043, 0.4027746460043180043, 0.4027746460043225007, 0.4027746460043225007, 0.4027746460043230003, 0.4027746460043230003, 0.4027746460043944987, 0.4027746460043944987, 0.4027746460042090360, 0.4027746460042090360, 0.4027746460044520083, 0.4027746460044520083, 0.4027746460044325238, 0.4027746460044325238),
 ( 0.4027746460044325238, 0.4027746460044325238, 0.4027746460044540067, 0.4027746460044540067, 0.4027746460044225318, 0.4027746460044225318, 0.4027746460043825083, 0.4027746460043825083, 0.4027746460043430399, 0.4027746460043430399, 0.4027746460043289956, 0.4027746460043289956, 0.4027746460043410415, 0.4027746460043410415, 0.4027746460044525079, 0.4027746460044525079, 0.4027746460044325238, 0.4027746460044325238, 0.4027746460044525079, 0.4027746460044525079, 0.4027746460043595267, 0.4027746460043595267, 0.4027746460044215326, 0.4027746460044215326, 0.4027746460043590271, 0.4027746460043590271, 0.4027746460044335230, 0.4027746460044335230, 0.4027746460043410415, 0.4027746460043410415, 0.4027746460042145316, 0.4027746460042145316, 0.4027746460044325238, 0.4027746460044325238, 0.4027746460044535071, 0.4027746460044535071, 0.4027746460044230314, 0.4027746460044230314, 0.4027746460043575283, 0.4027746460043575283, 0.4027746460043590271, 0.4027746460043590271, 0.4027746460043944987, 0.4027746460043944987, 0.4027746460043630239, 0.4027746460043630239, 0.4027746460044520083, 0.4027746460044520083, 0.4027746460044325238, 0.4027746460044325238, 0.4027746460044530075, 0.4027746460044530075, 0.4027746460043180043, 0.4027746460043180043, 0.4027746460043225007, 0.4027746460043225007, 0.4027746460043230003, 0.4027746460043230003, 0.4027746460043944987, 0.4027746460043944987, 0.4027746460042090360, 0.4027746460042090360, 0.4027746460044520083, 0.4027746460044520083, 0.4027746460044325238, 0.4027746460044325238),
 ( 1.000000000000000000, 1.000000000000000000, 1.000000000000000000, 1.000000000000000000, 1.000000000000000000, 1.000000000000000000, 1.000000000000000000, 1.000000000000000000, 1.000000000000000000, 1.000000000000000000, 1.000000000000000000, 1.000000000000000000, 1.000000000000000000, 1.000000000000000000, 1.000000000000000000, 1.000000000000000000, 1.000000000000000000, 1.000000000000000000, 1.000000000000000000, 1.000000000000000000, 1.000000000000000000, 1.000000000000000000, 1.000000000000000000, 1.000000000000000000, 1.000000000000000000, 1.000000000000000000, 1.000000000000000000, 1.000000000000000000, 1.000000000000000000, 1.000000000000000000, 1.000000000000000000, 1.000000000000000000, 1.000000000000000000, 1.000000000000000000, 1.000000000000000000, 1.000000000000000000, 1.000000000000000000, 1.000000000000000000, 1.000000000000000000, 1.000000000000000000, 1.000000000000000000, 1.000000000000000000, 1.000000000000000000, 1.000000000000000000, 1.000000000000000000, 1.000000000000000000, 1.000000000000000000, 1.000000000000000000, 1.000000000000000000, 1.000000000000000000, 1.000000000000000000, 1.000000000000000000, 1.000000000000000000, 1.000000000000000000, 1.000000000000000000, 1.000000000000000000, 1.000000000000000000, 1.000000000000000000, 1.000000000000000000, 1.000000000000000000, 1.000000000000000000, 1.000000000000000000, 1.000000000000000000, 1.000000000000000000, 1.000000000000000000, 1.000000000000000000) ) ) 
 REPRESENTATION_ITEM ( '' )  SURFACE ( )  );
#12448 = EDGE_LOOP ( 'NONE', ( #6058, #309, #3102, #6971 ) ) ;
#12449 = DIRECTION ( 'NONE',  ( 0.000000000000000000, 0.000000000000000000, 1.000000000000000000 ) ) ;
#12450 = EDGE_LOOP ( 'NONE', ( #9684, #9088, #2302, #249 ) ) ;
#12451 = CARTESIAN_POINT ( 'NONE',  ( 0.000000000000000000, 2.772967769359004908, 240.3921568627449972 ) ) ;
#12452 = CARTESIAN_POINT ( 'NONE',  ( -250.0000000000000000, -1.000000000000000000, -11.95826074310140008 ) ) ;
#12453 = CIRCLE ( 'NONE', #955, 6.500000000000005329 ) ;
#12454 = CARTESIAN_POINT ( 'NONE',  ( 206.8203823583192502, 20.08915143297736705, 158.7026972336032600 ) ) ;
#12455 = VERTEX_POINT ( 'NONE', #8475 ) ;
#12456 = CYLINDRICAL_SURFACE ( 'NONE', #11500, 4.000000000000000000 ) ;
#12457 = CARTESIAN_POINT ( 'NONE',  ( -243.5376947841724018, 7.773445842367202374, -9.141748602794347534 ) ) ;
#12458 = CARTESIAN_POINT ( 'NONE',  ( -239.5448319005391511, 1.867756356064017131, 11.85375772827623742 ) ) ;
#12459 = STYLED_ITEM ( 'NONE', ( #3928 ), #5911 ) ;
#12460 = SURFACE_SIDE_STYLE ('',( #10384 ) ) ;
#12461 = APPLICATION_PROTOCOL_DEFINITION ( 'draft international standard', 'automotive_design', 1998, #9515 ) ;
#12462 = CARTESIAN_POINT ( 'NONE',  ( -229.7397366602772877, 4.937265191653261276, -10.93887086792326002 ) ) ;
#12463 = FACE_OUTER_BOUND ( 'NONE', #6969, .T. ) ;
#12464 = ORIENTED_EDGE ( 'NONE', *, *, #3004, .T. ) ;
#12465 = CARTESIAN_POINT ( 'NONE',  ( -34.10614053579494964, 20.08915143303473982, -258.8746690718934929 ) ) ;
#12466 = DIRECTION ( 'NONE',  ( -0.000000000000000000, -1.000000000000000000, 0.000000000000000000 ) ) ;
#12467 = DIRECTION ( 'NONE',  ( -0.000000000000000000, -1.000000000000000000, 0.000000000000000000 ) ) ;
#12468 = AXIS2_PLACEMENT_3D ( 'NONE', #5509, #9569, #3503 ) ;
#12469 = EDGE_CURVE ( 'NONE', #4826, #204, #3825, .T. ) ;
#12470 = CARTESIAN_POINT ( 'NONE',  ( -249.4468820691694759, 10.72473315980031394, 4.809560401053397882 ) ) ;
#12471 = EDGE_CURVE ( 'NONE', #4062, #4661, #5969, .T. ) ;
#12472 = DIRECTION ( 'NONE',  ( 1.000000000000000000, 0.000000000000000000, 0.000000000000000000 ) ) ;
#12473 = DIRECTION ( 'NONE',  ( -0.000000000000000000, -1.000000000000000000, 0.000000000000000000 ) ) ;
#12474 = CARTESIAN_POINT ( 'NONE',  ( -246.1739743505053184, -9.287690276134259904, 7.598953578806062481 ) ) ;
#12475 = DIRECTION ( 'NONE',  ( -0.5887335932212929279, 0.5538822189107472926, 0.5887335932212909295 ) ) ;
#12476 = CARTESIAN_POINT ( 'NONE',  ( -248.0831933713610056, -9.830508068705269054, 6.436117704883859147 ) ) ;
#12477 = ORIENTED_EDGE ( 'NONE', *, *, #4479, .F. ) ;
#12478 = DIRECTION ( 'NONE',  ( 0.000000000000000000, 0.000000000000000000, 1.000000000000000000 ) ) ;
#12479 = CARTESIAN_POINT ( 'NONE',  ( -238.6985546758615442, -1.431921744593627863E-13, 12.00000000011287504 ) ) ;
#12480 = ORIENTED_EDGE ( 'NONE', *, *, #9152, .F. ) ;
#12481 = ORIENTED_EDGE ( 'NONE', *, *, #1628, .T. ) ;
#12482 = LINE ( 'NONE', #3274, #4017 ) ;
#12483 = DIRECTION ( 'NONE',  ( 1.000000000000000000, 0.000000000000000000, -1.224646799147353207E-16 ) ) ;
#12484 = CARTESIAN_POINT ( 'NONE',  ( -259.6535381480032356, 20.55460285108499008, 34.20858920320377905 ) ) ;
#12485 = FACE_OUTER_BOUND ( 'NONE', #437, .T. ) ;
#12486 = PRODUCT_DEFINITION_SHAPE ( 'NONE', 'NONE',  #13175 ) ;
#12487 = CARTESIAN_POINT ( 'NONE',  ( 0.000000000000000000, 0.000000000000000000, 0.000000000000000000 ) ) ;
#12488 = CARTESIAN_POINT ( 'NONE',  ( -240.6798348123334108, 4.210664053274118857, 10.96963869245110601 ) ) ;
#12489 = CARTESIAN_POINT ( 'NONE',  ( -158.8368823490027921, 20.79694577634646535, 206.9952515782965179 ) ) ;
#12490 = EDGE_LOOP ( 'NONE', ( #516, #12026 ) ) ;
#12491 = FACE_OUTER_BOUND ( 'NONE', #4279, .T. ) ;
#12492 = ADVANCED_FACE ( 'NONE', ( #1467 ), #1908, .F. ) ;
#12493 = ORIENTED_EDGE ( 'NONE', *, *, #11847, .T. ) ;
#12494 = ADVANCED_FACE ( 'NONE', ( #1407 ), #7458, .F. ) ;
#12495 = DIRECTION ( 'NONE',  ( 0.000000000000000000, 0.9998057603070480415, -0.01970892327970899874 ) ) ;
#12496 = VERTEX_POINT ( 'NONE', #8731 ) ;
#12497 = ORIENTED_EDGE ( 'NONE', *, *, #7872, .F. ) ;
#12498 = CARTESIAN_POINT ( 'NONE',  ( 0.000000000000000000, 30.00000000000000000, 0.000000000000000000 ) ) ;
#12499 = CARTESIAN_POINT ( 'NONE',  ( -197.8197553893924976, 19.00000000000000000, -58.77553482998720114 ) ) ;
#12500 = DIRECTION ( 'NONE',  ( 0.000000000000000000, 1.000000000000000000, 0.000000000000000000 ) ) ;
#12501 = CARTESIAN_POINT ( 'NONE',  ( 238.9743709119393316, 0.1785824617006206982, -3.500006748978118587 ) ) ;
#12502 = DIRECTION ( 'NONE',  ( -0.000000000000000000, -1.000000000000000000, 0.000000000000000000 ) ) ;
#12503 = CARTESIAN_POINT ( 'NONE',  ( -242.2936178120088755, 6.614827066046929716, 10.01219624234327021 ) ) ;
#12504 = FILL_AREA_STYLE ('',( #11513 ) ) ;
#12505 = CONTEXT_DEPENDENT_SHAPE_REPRESENTATION ( #8039, #9401 ) ;
#12506 = EDGE_LOOP ( 'NONE', ( #3722, #3993, #3220, #486 ) ) ;
#12507 = FACE_OUTER_BOUND ( 'NONE', #12732, .T. ) ;
#12509 = EDGE_LOOP ( 'NONE', ( #2900, #6288 ) ) ;
#12508 = AXIS2_PLACEMENT_3D ( 'NONE', #10455, #3312, #9516 ) ;
#12510 = EDGE_CURVE ( 'NONE', #8290, #7801, #12789, .T. ) ;
#12511 = DIRECTION ( 'NONE',  ( -0.000000000000000000, 1.000000000000000000, 0.000000000000000000 ) ) ;
#12512 = DIRECTION ( 'NONE',  ( 0.000000000000000000, 0.9998057603070481525, -0.01970892327970900221 ) ) ;
#12513 = CARTESIAN_POINT ( 'NONE',  ( 190.2689011420771976, 20.08915143297736350, -178.2104428091926991 ) ) ;
#12514 = ORIENTED_EDGE ( 'NONE', *, *, #12397, .T. ) ;
#12515 = EDGE_CURVE ( 'NONE', #534, #7886, #11505, .T. ) ;
#12516 = DIRECTION ( 'NONE',  ( -1.000000000000000000, -0.000000000000000000, -0.000000000000000000 ) ) ;
#12517 = CARTESIAN_POINT ( 'NONE',  ( -244.8348239360272771, 8.646460184776158187, -8.320981818718424350 ) ) ;
#12518 = CARTESIAN_POINT ( 'NONE',  ( -239.1309277283428685, 1.402640123932128891, 11.91796374952781790 ) ) ;
#12519 = CARTESIAN_POINT ( 'NONE',  ( -240.6673884782285029, -4.184756593312895845, -10.97954905606168907 ) ) ;
#12520 = AXIS2_PLACEMENT_3D ( 'NONE', #2419, #12684, #8494 ) ;
#12521 = SHAPE_REPRESENTATION ( 'Grease Lubrication Injection Nipple', ( #805 ), #5055 ) ;
#12522 = CARTESIAN_POINT ( 'NONE',  ( 239.5494890104657770, -1.589230969769584556, 3.118420702999415095 ) ) ;
#12523 = CARTESIAN_POINT ( 'NONE',  ( 240.5500529090693078, 3.279976618980518843, 1.225241158572545785 ) ) ;
#12524 = AXIS2_PLACEMENT_3D ( 'NONE', #3078, #7159, #97 ) ;
#12525 = AXIS2_PLACEMENT_3D ( 'NONE', #5342, #280, #8611 ) ;
#12526 = DIRECTION ( 'NONE',  ( 0.000000000000000000, 1.000000000000000000, 0.000000000000000000 ) ) ;
#12527 = ORIENTED_EDGE ( 'NONE', *, *, #306, .F. ) ;
#12528 = CARTESIAN_POINT ( 'NONE',  ( 159.3024069661366866, 19.96883746137792670, -207.6469600131167681 ) ) ;
#12529 = DIRECTION ( 'NONE',  ( 0.6368676505102700558, 0.000000000000000000, 0.7709731485165541853 ) ) ;
#12530 = CARTESIAN_POINT ( 'NONE',  ( -0.000000000000000000, -3.061616997868385015E-14, 0.000000000000000000 ) ) ;
#12531 = CARTESIAN_POINT ( 'NONE',  ( -233.0000000000000000, 1.000000000000000000, -12.50000000000000000 ) ) ;
#12532 = DIRECTION ( 'NONE',  ( -0.000000000000000000, -1.000000000000000000, 0.000000000000000000 ) ) ;
#12533 = CIRCLE ( 'NONE', #7850, 3.000000000000000000 ) ;
#12534 = LINE ( 'NONE', #5341, #9438 ) ;
#12535 = DIRECTION ( 'NONE',  ( -0.8199460427888396463, 0.5538822189107472926, -0.1445786100688130904 ) ) ;
#12536 = CIRCLE ( 'NONE', #9978, 6.500000000000000888 ) ;
#12537 = CARTESIAN_POINT ( 'NONE',  ( -293.9524689910264215, -18.00000000000000000, 5.406159583508754807 ) ) ;
#12538 = VECTOR ( 'NONE', #5420, 1000.000000000000114 ) ;
#12539 = FACE_OUTER_BOUND ( 'NONE', #11904, .T. ) ;
#12540 = CIRCLE ( 'NONE', #6801, 249.7999999999999829 ) ;
#12541 = EDGE_CURVE ( 'NONE', #2702, #4133, #645, .T. ) ;
#12542 = CARTESIAN_POINT ( 'NONE',  ( -229.9555022783201821, -11.11474285528676376, 4.527357793578296707 ) ) ;
#12543 = ORIENTED_EDGE ( 'NONE', *, *, #1510, .T. ) ;
#12544 = ORIENTED_EDGE ( 'NONE', *, *, #8940, .T. ) ;
#12545 = AXIS2_PLACEMENT_3D ( 'NONE', #9768, #5647, #10712 ) ;
#12546 = CYLINDRICAL_SURFACE ( 'NONE', #11887, 239.0000000000000000 ) ;
#12547 = FACE_BOUND ( 'NONE', #1827, .T. ) ;
#12548 = TOROIDAL_SURFACE ( 'NONE', #5309, 252.1999999999999886, 2.000000000000000000 ) ;
#12549 = CARTESIAN_POINT ( 'NONE',  ( -252.9796497731091165, 20.55460285134058651, -67.76049180360037383 ) ) ;
#12550 = LINE ( 'NONE', #298, #9844 ) ;
#12551 =( REPRESENTATION_RELATIONSHIP ('NONE','NONE', #12019, #182 ) REPRESENTATION_RELATIONSHIP_WITH_TRANSFORMATION ( #9846 )SHAPE_REPRESENTATION_RELATIONSHIP( ) );
#12552 = DIRECTION ( 'NONE',  ( -0.9396926207859069846, 0.000000000000000000, -0.3420201433256726542 ) ) ;
#12553 = FACE_OUTER_BOUND ( 'NONE', #762, .T. ) ;
#12554 = CARTESIAN_POINT ( 'NONE',  ( -239.9450917581429792, -2.156506209390995021, -11.80463811257499884 ) ) ;
#12555 = AXIS2_PLACEMENT_3D ( 'NONE', #2558, #9746, #10072 ) ;
#12556 = ORIENTED_EDGE ( 'NONE', *, *, #4765, .T. ) ;
#12557 = EDGE_CURVE ( 'NONE', #3301, #379, #2344, .T. ) ;
#12558 = CARTESIAN_POINT ( 'NONE',  ( -11.00000000000000000, 0.000000000000000000, 250.0000000000000000 ) ) ;
#12559 = EDGE_CURVE ( 'NONE', #5655, #6838, #10470, .T. ) ;
#12560 = AXIS2_PLACEMENT_3D ( 'NONE', #10576, #5576, #2311 ) ;
#12561 = ORIENTED_EDGE ( 'NONE', *, *, #7386, .F. ) ;
#12562 = DIRECTION ( 'NONE',  ( -0.000000000000000000, -1.000000000000000000, 0.000000000000000000 ) ) ;
#12563 = ORIENTED_EDGE ( 'NONE', *, *, #4159, .T. ) ;
#12564 = VERTEX_POINT ( 'NONE', #6541 ) ;
#12565 = CARTESIAN_POINT ( 'NONE',  ( 0.000000000000000000, 0.000000000000000000, 0.000000000000000000 ) ) ;
#12566 = PRODUCT_DEFINITION_SHAPE ( 'NONE', 'NONE',  #5139 ) ;
#12567 = CARTESIAN_POINT ( 'NONE',  ( 181.8257142206846311, -18.00000000000000000, 220.1128339014740618 ) ) ;
#12568 =( REPRESENTATION_RELATIONSHIP ('NONE','NONE', #12019, #182 ) REPRESENTATION_RELATIONSHIP_WITH_TRANSFORMATION ( #4339 )SHAPE_REPRESENTATION_RELATIONSHIP( ) );
#12569 = EDGE_CURVE ( 'NONE', #779, #11069, #5530, .T. ) ;
#12570 = FACE_OUTER_BOUND ( 'NONE', #12156, .T. ) ;
#12571 = AXIS2_PLACEMENT_3D ( 'NONE', #7068, #6131, #10183 ) ;
#12572 = CARTESIAN_POINT ( 'NONE',  ( -239.1938287653389636, 1.469862578567988853, -11.65770166428045584 ) ) ;
#12573 = DIRECTION ( 'NONE',  ( -0.000000000000000000, -1.000000000000000000, 0.000000000000000000 ) ) ;
#12574 = VECTOR ( 'NONE', #7604, 1000.000000000000000 ) ;
#12575 = ORIENTED_EDGE ( 'NONE', *, *, #3049, .T. ) ;
#12576 = CYLINDRICAL_SURFACE ( 'NONE', #6471, 3.499999999999964917 ) ;
#12577 = ORIENTED_EDGE ( 'NONE', *, *, #938, .T. ) ;
#12578 = CARTESIAN_POINT ( 'NONE',  ( -244.0310755671143284, 8.130894654072220007, -8.482269552766895870 ) ) ;
#12579 = DIRECTION ( 'NONE',  ( 0.000000000000000000, 1.000000000000000000, 0.000000000000000000 ) ) ;
#12580 =( GEOMETRIC_REPRESENTATION_CONTEXT ( 3 ) GLOBAL_UNCERTAINTY_ASSIGNED_CONTEXT ( ( #5354 ) ) GLOBAL_UNIT_ASSIGNED_CONTEXT ( ( #7526, #5456, #12652 ) ) REPRESENTATION_CONTEXT ( 'NONE', 'WORKASPACE' ) );
#12581 = CARTESIAN_POINT ( 'NONE',  ( 258.4638482596385529, 20.08915143297736350, 34.02434144668556115 ) ) ;
#12582 = DIRECTION ( 'NONE',  ( -1.000000000000000000, 0.000000000000000000, 0.000000000000000000 ) ) ;
#12583 = CARTESIAN_POINT ( 'NONE',  ( -242.1181102628582664, 6.423496681710723522, -10.13942498697665862 ) ) ;
#12584 = DIRECTION ( 'NONE',  ( 8.659560562354913137E-17, -0.7071067811865489050, 0.7071067811865460184 ) ) ;
#12585 = EDGE_CURVE ( 'NONE', #2601, #5508, #1709, .T. ) ;
#12586 = CARTESIAN_POINT ( 'NONE',  ( 197.8197553893920144, 19.00000000000000000, 64.27553482998850143 ) ) ;
#12587 = EDGE_CURVE ( 'NONE', #12985, #4948, #11736, .T. ) ;
#12588 = CARTESIAN_POINT ( 'NONE',  ( -245.4297298679771586, -8.960803861643656276, 7.981710862397758177 ) ) ;
#12589 = DIRECTION ( 'NONE',  ( 0.000000000000000000, -0.7071067811865489050, -0.7071067811865460184 ) ) ;
#12590 = CARTESIAN_POINT ( 'NONE',  ( -229.8945924270675221, 9.781573351764743407, -6.991165551757859475 ) ) ;
#12591 = ADVANCED_FACE ( 'NONE', ( #8662, #3592 ), #6802, .F. ) ;
#12592 = AXIS2_PLACEMENT_3D ( 'NONE', #646, #4698, #7832 ) ;
#12593 = LINE ( 'NONE', #11666, #8073 ) ;
#12594 = ORIENTED_EDGE ( 'NONE', *, *, #4626, .F. ) ;
#12595 = PRODUCT_DEFINITION_SHAPE ( 'NONE', 'NONE',  #13117 ) ;
#12596 = CARTESIAN_POINT ( 'NONE',  ( -1.008906662707803564E-12, 19.96883746059272724, 261.1558126970361400 ) ) ;
#12597 = CARTESIAN_POINT ( 'NONE',  ( -0.000000000000000000, -25.00000000000000000, 0.000000000000000000 ) ) ;
#12598 = CARTESIAN_POINT ( 'NONE',  ( 181.8257142206846311, -30.00000000000000000, 220.1128339014740618 ) ) ;
#12599 = DIRECTION ( 'NONE',  ( 0.000000000000000000, 0.000000000000000000, -1.000000000000000000 ) ) ;
#12600 = ADVANCED_FACE ( 'NONE', ( #12002 ), #2848, .T. ) ;
#12601 = CARTESIAN_POINT ( 'NONE',  ( -260.1353576186481291, 20.08915143297736705, -17.05322212017824768 ) ) ;
#12602 = CARTESIAN_POINT ( 'NONE',  ( 71.82423009839129691, 30.00000000000000000, 192.2354503650404922 ) ) ;
#12603 = DIRECTION ( 'NONE',  ( 0.9659258262890680902, 0.000000000000000000, 0.2588190451025213501 ) ) ;
#12604 = DIRECTION ( 'NONE',  ( 0.000000000000000000, 1.000000000000000000, 0.000000000000000000 ) ) ;
#12605 = AXIS2_PLACEMENT_3D ( 'NONE', #8604, #3589, #7657 ) ;
#12606 = CARTESIAN_POINT ( 'NONE',  ( -240.4767932493553531, -3.790394256708240484, -11.38565896274289280 ) ) ;
#12607 = CARTESIAN_POINT ( 'NONE',  ( -229.6889200636375108, -1.000000000000000000, 11.95826074310140008 ) ) ;
#12608 = AXIS2_PLACEMENT_3D ( 'NONE', #10717, #6212, #5649 ) ;
#12609 = ORIENTED_EDGE ( 'NONE', *, *, #3286, .T. ) ;
#12610 = VERTEX_POINT ( 'NONE', #11861 ) ;
#12611 = CARTESIAN_POINT ( 'NONE',  ( 0.000000000000000000, 4.286263797015693701E-16, -3.499999999999964917 ) ) ;
#12612 = CARTESIAN_POINT ( 'NONE',  ( 290.6841825403032544, -19.00000000000000000, 27.68945685411186730 ) ) ;
#12613 = AXIS2_PLACEMENT_3D ( 'NONE', #4408, #10349, #5482 ) ;
#12614 = CARTESIAN_POINT ( 'NONE',  ( 234.7354397747064354, 19.96883745941838484, 115.7315435904383349 ) ) ;
#12615 = LINE ( 'NONE', #3479, #906 ) ;
#12616 = DIRECTION ( 'NONE',  ( -0.9659258262890690894, 0.000000000000000000, 0.2588190451025179639 ) ) ;
#12617 = MECHANICAL_DESIGN_GEOMETRIC_PRESENTATION_REPRESENTATION (  '', ( #3677 ), #6452 ) ;
#12618 = DIRECTION ( 'NONE',  ( 0.000000000000000000, 0.000000000000000000, 1.000000000000000000 ) ) ;
#12619 = DIRECTION ( 'NONE',  ( -0.000000000000000000, 1.000000000000000000, 0.000000000000000000 ) ) ;
#12620 = ORIENTED_EDGE ( 'NONE', *, *, #200, .F. ) ;
#12621 = CARTESIAN_POINT ( 'NONE',  ( 42.50473797389777530, 20.79694577634646890, -257.4287020129718826 ) ) ;
#12622 = ORIENTED_EDGE ( 'NONE', *, *, #4011, .T. ) ;
#12623 = DIRECTION ( 'NONE',  ( -0.000000000000000000, 1.000000000000000000, 0.000000000000000000 ) ) ;
#12624 = ORIENTED_EDGE ( 'NONE', *, *, #12061, .F. ) ;
#12625 = ORIENTED_EDGE ( 'NONE', *, *, #4801, .T. ) ;
#12626 = AXIS2_PLACEMENT_3D ( 'NONE', #11006, #949, #7149 ) ;
#12627 = TOROIDAL_SURFACE ( 'NONE', #7946, 238.4705882352940307, 2.000000000000000000 ) ;
#12628 = AXIS2_PLACEMENT_3D ( 'NONE', #7679, #4605, #8680 ) ;
#12629 = CIRCLE ( 'NONE', #6464, 5.500000000000015099 ) ;
#12630 = DIRECTION ( 'NONE',  ( 0.000000000000000000, -1.000000000000000000, 0.000000000000000000 ) ) ;
#12631 = CARTESIAN_POINT ( 'NONE',  ( -31.19222893191935242, -30.00000000000000000, 286.4438302234617595 ) ) ;
#12632 = AXIS2_PLACEMENT_3D ( 'NONE', #753, #11945, #11878 ) ;
#12633 = ADVANCED_FACE ( 'NONE', ( #1731 ), #10, .F. ) ;
#12634 = EDGE_CURVE ( 'NONE', #8176, #12433, #5323, .T. ) ;
#12635 = CARTESIAN_POINT ( 'NONE',  ( -122.2593324768359935, 30.00000000000000000, -162.7755348299880040 ) ) ;
#12636 = DIRECTION ( 'NONE',  ( 0.6368676505102707219, 0.000000000000000000, 0.7709731485165535192 ) ) ;
#12637 = CARTESIAN_POINT ( 'NONE',  ( -130.7196491263533744, -20.69999999999999929, 200.0834159351620656 ) ) ;
#12638 = AXIS2_PLACEMENT_3D ( 'NONE', #12095, #2954, #12035 ) ;
#12639 = EDGE_LOOP ( 'NONE', ( #8009, #3683 ) ) ;
#12640 = AXIS2_PLACEMENT_3D ( 'NONE', #2587, #10730, #5334 ) ;
#12641 = CARTESIAN_POINT ( 'NONE',  ( -238.7275296710179191, -0.3340951308803304376, 11.74628516890670760 ) ) ;
#12642 = ORIENTED_EDGE ( 'NONE', *, *, #3708, .T. ) ;
#12643 = DIRECTION ( 'NONE',  ( 0.6368676505102707219, 0.000000000000000000, 0.7709731485165535192 ) ) ;
#12644 = CARTESIAN_POINT ( 'NONE',  ( 159.3442861576696998, 0.000000000000000000, 192.8974817588416784 ) ) ;
#12645 = AXIS2_PLACEMENT_3D ( 'NONE', #13029, #968, #6968 ) ;
#12646 = CARTESIAN_POINT ( 'NONE',  ( 235.4000000000000057, 0.000000000000000000, 0.000000000000000000 ) ) ;
#12647 = DIRECTION ( 'NONE',  ( 1.000000000000000000, 0.000000000000000000, 0.000000000000000000 ) ) ;
#12648 = CARTESIAN_POINT ( 'NONE',  ( -239.2285245180114828, 1.532942925007542145, 11.90165677312966785 ) ) ;
#12649 = CARTESIAN_POINT ( 'NONE',  ( -240.1208361041844910, -2.772967769359084844, -11.41810622433049893 ) ) ;
#12650 = VECTOR ( 'NONE', #68, 1000.000000000000000 ) ;
#12651 = DIRECTION ( 'NONE',  ( 0.000000000000000000, 0.000000000000000000, -1.000000000000000000 ) ) ;
#12652 =( NAMED_UNIT ( * ) SI_UNIT ( $, .STERADIAN. ) SOLID_ANGLE_UNIT ( ) );
#12653 = CARTESIAN_POINT ( 'NONE',  ( 0.000000000000000000, 29.00000000000000000, 0.000000000000000000 ) ) ;
#12654 = CONTEXT_DEPENDENT_SHAPE_REPRESENTATION ( #11585, #2688 ) ;
#12655 = AXIS2_PLACEMENT_3D ( 'NONE', #7462, #12396, #11461 ) ;
#12656 = EDGE_CURVE ( 'NONE', #1432, #7625, #7030, .T. ) ;
#12657 = EDGE_CURVE ( 'NONE', #4193, #3121, #12300, .T. ) ;
#12658 = LINE ( 'NONE', #7590, #12972 ) ;
#12659 = VERTEX_POINT ( 'NONE', #739 ) ;
#12660 =( REPRESENTATION_RELATIONSHIP ('NONE','NONE', #12019, #5191 ) REPRESENTATION_RELATIONSHIP_WITH_TRANSFORMATION ( #8005 )SHAPE_REPRESENTATION_RELATIONSHIP( ) );
#12661 = CARTESIAN_POINT ( 'NONE',  ( -226.6392846543355688, 19.96883746039994278, 130.8783844631124680 ) ) ;
#12662 = DIRECTION ( 'NONE',  ( 0.000000000000000000, 1.000000000000000000, 0.000000000000000000 ) ) ;
#12663 = CARTESIAN_POINT ( 'NONE',  ( 3.046921236278614777E-14, -20.00000000000000000, -248.7999999999999829 ) ) ;
#12664 = CARTESIAN_POINT ( 'NONE',  ( -1.008906662707803362E-12, 19.96883746059273435, 261.1558126970361400 ) ) ;
#12665 = PRESENTATION_LAYER_ASSIGNMENT (  '', '', ( #3288 ) ) ;
#12666 = CARTESIAN_POINT ( 'NONE',  ( -107.5873595010545500, 20.08915143297736705, 237.4577367525701845 ) ) ;
#12667 = DIRECTION ( 'NONE',  ( 0.000000000000000000, 0.000000000000000000, 1.000000000000000000 ) ) ;
#12668 = CARTESIAN_POINT ( 'NONE',  ( -32.05991134143130949, -138.4705547276867321, 26.90145978217120870 ) ) ;
#12669 = CARTESIAN_POINT ( 'NONE',  ( -229.7741891532738236, -5.886256761507725699, -10.19824341982703331 ) ) ;
#12670 = ITEM_DEFINED_TRANSFORMATION ( 'NONE', 'NONE', #229,  #805 ) ;
#12671 = DIRECTION ( 'NONE',  ( 0.000000000000000000, -1.000000000000000000, 0.000000000000000000 ) ) ;
#12672 = AXIS2_PLACEMENT_3D ( 'NONE', #5584, #6527, #7780 ) ;
#12673 = EDGE_CURVE ( 'NONE', #9146, #6953, #4787, .T. ) ;
#12674 = AXIS2_PLACEMENT_3D ( 'NONE', #170, #7168, #9166 ) ;
#12675 = CARTESIAN_POINT ( 'NONE',  ( -229.7802203235890204, -6.580825742931379452, 10.06232612585050035 ) ) ;
#12676 = VERTEX_POINT ( 'NONE', #4716 ) ;
#12677 = ORIENTED_EDGE ( 'NONE', *, *, #3097, .T. ) ;
#12678 = CARTESIAN_POINT ( 'NONE',  ( -185.9653539489998195, -19.00000000000000000, -225.1241593668329699 ) ) ;
#12679 = FACE_BOUND ( 'NONE', #1496, .T. ) ;
#12680 = ADVANCED_FACE ( 'NONE', ( #8796 ), #863, .F. ) ;
#12681 = CARTESIAN_POINT ( 'NONE',  ( -17.06760680892479698, 20.79694577614318973, 260.7745447066434963 ) ) ;
#12682 = CONICAL_SURFACE ( 'NONE', #6310, 6.500000000000005329, 0.7853981633974476129 ) ;
#12683 = FACE_OUTER_BOUND ( 'NONE', #8214, .T. ) ;
#12684 = DIRECTION ( 'NONE',  ( -0.9396926207859093161, 0.000000000000000000, 0.3420201433256663259 ) ) ;
#12685 = CARTESIAN_POINT ( 'NONE',  ( -249.7118339206215012, 9.997999799959989886, 6.636264009214830395 ) ) ;
#12686 = FACE_OUTER_BOUND ( 'NONE', #3565, .T. ) ;
#12687 = ORIENTED_EDGE ( 'NONE', *, *, #3607, .F. ) ;
#12688 = CARTESIAN_POINT ( 'NONE',  ( 247.0684411393755795, 20.79694577634646535, -83.86521783953189413 ) ) ;
#12689 = ORIENTED_EDGE ( 'NONE', *, *, #5789, .F. ) ;
#12690 = CARTESIAN_POINT ( 'NONE',  ( -0.000000000000000000, -3.061616997868385015E-14, 0.000000000000000000 ) ) ;
#12691 = EDGE_LOOP ( 'NONE', ( #6836, #12622, #94, #3828 ) ) ;
#12692 = ORIENTED_EDGE ( 'NONE', *, *, #12422, .T. ) ;
#12693 = CARTESIAN_POINT ( 'NONE',  ( 233.5975020798683204, 2.999417280921144346, -0.05912676983912699968 ) ) ;
#12694 = CARTESIAN_POINT ( 'NONE',  ( 239.0028278883881399, -0.3789072388328452168, -3.479912193147403521 ) ) ;
#12695 = DIRECTION ( 'NONE',  ( -0.000000000000000000, -1.000000000000000000, 0.000000000000000000 ) ) ;
#12696 = FACE_OUTER_BOUND ( 'NONE', #9545, .T. ) ;
#12697 = FACE_OUTER_BOUND ( 'NONE', #574, .T. ) ;
#12698 = CONTEXT_DEPENDENT_SHAPE_REPRESENTATION ( #5933, #915 ) ;
#12699 = ORIENTED_EDGE ( 'NONE', *, *, #12916, .F. ) ;
#12700 = B_SPLINE_CURVE_WITH_KNOTS ( 'NONE', 3,
 ( #4923, #9996, #3725, #7792, #6067, #12195, #3048, #9324, #10180, #4055, #196, #7133, #3983, #11188, #8134, #2189, #10120, #3113, #1197, #10381, #3246, #4253, #2055, #12264, #5183, #11325, #993, #5045, #71, #6269, #1058, #6125, #7327, #4123, #9122, #2982, #1259, #5117, #1996, #7190, #11396, #8204, #11257, #9263, #10318, #9193, #5322, #136, #6197, #2119, #9392, #8060, #8266, #12329, #4186, #10250, #5255, #2256, #8333, #1126, #6330, #3179, #12126, #7261, #12391, #7063, #13040, #11123, #5453, #7390, #4507, #7644, #2448, #5580, #1517, #11530, #12519, #390, #8592, #7456, #12649 ),
 .UNSPECIFIED., .F., .F.,
 ( 4, 1, 1, 1, 2, 2, 2, 1, 1, 1, 2, 2, 2, 2, 1, 1, 1, 1, 2, 2, 2, 2, 1, 1, 1, 2, 2, 2, 1, 1, 1, 2, 2, 2, 2, 1, 1, 1, 2, 2, 2, 1, 1, 1, 2, 2, 2, 1, 1, 1, 2, 2, 4 ),
 ( 0.000000000000000000, 0.03125000000017429114, 0.04687500000026457309, 0.05468750000030974528, 0.05859375000032932684, 0.06250000000034891534, 0.09375000000051852966, 0.1093750000006062650, 0.1171875000006501188, 0.1210937500006691869, 0.1230468750006787210, 0.1250000000006882550, 0.1875000000008141265, 0.2187500000008799350, 0.2343750000009128254, 0.2421875000009293399, 0.2460937500009350576, 0.2480468750009355017, 0.2490234375009333367, 0.2500000000009311441, 0.3125000000007751577, 0.3437500000006971645, 0.3593750000006558087, 0.3671875000006373790, 0.3710937500006282752, 0.3730468750006217249, 0.3750000000006151746, 0.4375000000005053180, 0.4687500000004528045, 0.4843750000004288792, 0.4921875000004191647, 0.4960937500004121703, 0.5000000000004051204, 0.5625000000002996492, 0.5937500000002491340, 0.6093750000002217115, 0.6171875000002102762, 0.6210937500002069456, 0.6230468750002076117, 0.6250000000002082778, 0.6875000000001613154, 0.7187500000001358913, 0.7343750000001232348, 0.7421875000001169065, 0.7460937500001155742, 0.7500000000001142419, 0.8125000000000828226, 0.8437500000000686118, 0.8593750000000600631, 0.8671875000000571765, 0.8710937500000570655, 0.8750000000000569544, 1.000000000000000000 ),
 .UNSPECIFIED. ) ;
#12701 = CARTESIAN_POINT ( 'NONE',  ( -238.8961190158434817, -0.9395161414439207048, 11.71239737841137796 ) ) ;
#12702 = VERTEX_POINT ( 'NONE', #12924 ) ;
#12703 = CARTESIAN_POINT ( 'NONE',  ( -240.8355308712237104, 4.526241345699689944, -10.84528472040825875 ) ) ;
#12704 = CARTESIAN_POINT ( 'NONE',  ( 0.000000000000000000, 30.00000000000000000, -201.4999999999999716 ) ) ;
#12705 = ADVANCED_FACE ( 'NONE', ( #7860 ), #4836, .T. ) ;
#12706 = DIRECTION ( 'NONE',  ( -0.000000000000000000, 1.000000000000000000, 0.000000000000000000 ) ) ;
#12707 = CARTESIAN_POINT ( 'NONE',  ( 290.6841825403032544, -19.00000000000000000, 27.68945685411186730 ) ) ;
#12708 = CARTESIAN_POINT ( 'NONE',  ( -238.7400358149041324, 0.4567369020058948959, 11.99149615616909514 ) ) ;
#12709 = DIRECTION ( 'NONE',  ( 0.000000000000000000, -1.000000000000000000, 0.000000000000000000 ) ) ;
#12710 = CARTESIAN_POINT ( 'NONE',  ( -249.0734550459510785, -9.965425394270200243, 6.685150203391385659 ) ) ;
#12711 = CIRCLE ( 'NONE', #4827, 240.2352941176469869 ) ;
#12712 = FACE_OUTER_BOUND ( 'NONE', #5026, .T. ) ;
#12713 = CARTESIAN_POINT ( 'NONE',  ( -229.7895871136148003, 6.880706567532733686, 9.838484686103685206 ) ) ;
#12714 = CONTEXT_DEPENDENT_SHAPE_REPRESENTATION ( #597, #7924 ) ;
#12715 = EDGE_LOOP ( 'NONE', ( #8310, #8690, #1763, #3994 ) ) ;
#12716 = DIRECTION ( 'NONE',  ( 0.000000000000000000, 0.000000000000000000, 1.000000000000000000 ) ) ;
#12717 = ORIENTED_EDGE ( 'NONE', *, *, #3940, .T. ) ;
#12718 = CARTESIAN_POINT ( 'NONE',  ( 259.4723857435292302, 19.96883745945557820, -34.18476129351679305 ) ) ;
#12719 = CARTESIAN_POINT ( 'NONE',  ( 229.9000000000000057, 0.1024105694487990187, 5.195143123655512341 ) ) ;
#12720 = CARTESIAN_POINT ( 'NONE',  ( -248.0831933713610056, -9.830508068705269054, 6.436117704883859147 ) ) ;
#12721 = CARTESIAN_POINT ( 'NONE',  ( -293.9524689910264215, -30.00000000000000000, 5.406159583508762800 ) ) ;
#12722 = CARTESIAN_POINT ( 'NONE',  ( -241.1581829740684668, 5.108108803741933102, 10.85886904359302818 ) ) ;
#12723 = EDGE_CURVE ( 'NONE', #5558, #4886, #12711, .T. ) ;
#12724 = ADVANCED_FACE ( 'NONE', ( #798 ), #1223, .F. ) ;
#12725 = FACE_OUTER_BOUND ( 'NONE', #11517, .T. ) ;
#12726 = DIRECTION ( 'NONE',  ( -0.7823834078220635035, 0.5538822189107471816, 0.2847642722309838836 ) ) ;
#12727 = DIRECTION ( 'NONE',  ( 8.659560562354913137E-17, -0.7071067811865489050, 0.7071067811865460184 ) ) ;
#12728 = AXIS2_PLACEMENT_3D ( 'NONE', #9606, #6560, #4604 ) ;
#12729 = FACE_OUTER_BOUND ( 'NONE', #2142, .T. ) ;
#12730 = CARTESIAN_POINT ( 'NONE',  ( 122.2593324768346008, 30.00000000000000000, 161.7755348299889988 ) ) ;
#12731 = ORIENTED_EDGE ( 'NONE', *, *, #5835, .F. ) ;
#12732 = EDGE_LOOP ( 'NONE', ( #12121, #3348, #4484, #12766 ) ) ;
#12733 = CARTESIAN_POINT ( 'NONE',  ( 234.4000000000000057, 3.999223041228189057, -0.07883569311883543984 ) ) ;
#12734 = FACE_OUTER_BOUND ( 'NONE', #6568, .T. ) ;
#12735 = AXIS2_PLACEMENT_3D ( 'NONE', #6188, #11242, #12384 ) ;
#12736 = CIRCLE ( 'NONE', #12964, 5.499999999999986677 ) ;
#12737 = CIRCLE ( 'NONE', #8701, 250.7000000000000171 ) ;
#12738 = EDGE_CURVE ( 'NONE', #10046, #5784, #799, .T. ) ;
#12739 = CARTESIAN_POINT ( 'NONE',  ( 172.6991790967991847, 20.55460285078499183, -196.8887528227133714 ) ) ;
#12740 = AXIS2_PLACEMENT_3D ( 'NONE', #3009, #9891, #891 ) ;
#12741 = EDGE_CURVE ( 'NONE', #4661, #10245, #10881, .T. ) ;
#12742 = CARTESIAN_POINT ( 'NONE',  ( -197.8197553893924976, 19.00000000000000000, -64.27553482998719403 ) ) ;
#12743 = DIRECTION ( 'NONE',  ( -0.5735764363510416075, 0.000000000000000000, -0.8191520442889949072 ) ) ;
#12744 = CARTESIAN_POINT ( 'NONE',  ( 239.7985776503625175, 1.848645179571945185, 2.971954070985139751 ) ) ;
#12745 = AXIS2_PLACEMENT_3D ( 'NONE', #4713, #2525, #6603 ) ;
#12746 = CARTESIAN_POINT ( 'NONE',  ( 239.9471905437599730, 1.993882481326073375, -2.878173188143535732 ) ) ;
#12747 = AXIS2_PLACEMENT_3D ( 'NONE', #591, #7787, #12987 ) ;
#12748 = EDGE_LOOP ( 'NONE', ( #969, #10973, #5658, #9782 ) ) ;
#12749 = CARTESIAN_POINT ( 'NONE',  ( 0.000000000000000000, -11.79660968244690089, 0.000000000000000000 ) ) ;
#12750 = EDGE_CURVE ( 'NONE', #2005, #10427, #5046, .T. ) ;
#12751 = AXIS2_PLACEMENT_3D ( 'NONE', #12172, #12244, #3095 ) ;
#12752 = CARTESIAN_POINT ( 'NONE',  ( 164.6302876569049829, -3.165711975795909891E-14, 199.2965588915290880 ) ) ;
#12753 = ORIENTED_EDGE ( 'NONE', *, *, #2479, .F. ) ;
#12754 = ORIENTED_EDGE ( 'NONE', *, *, #6457, .F. ) ;
#12755 = EDGE_LOOP ( 'NONE', ( #12813, #8898 ) ) ;
#12756 = AXIS2_PLACEMENT_3D ( 'NONE', #9215, #6893, #12478 ) ;
#12757 = DIRECTION ( 'NONE',  ( 0.000000000000000000, 1.000000000000000000, 0.000000000000000000 ) ) ;
#12758 = DIRECTION ( 'NONE',  ( 0.6368676505102700558, 0.000000000000000000, 0.7709731485165541853 ) ) ;
#12759 = CARTESIAN_POINT ( 'NONE',  ( -83.95474316008289861, 20.08915143298712280, -247.2466869553079789 ) ) ;
#12760 = AXIS2_PLACEMENT_3D ( 'NONE', #2679, #6640, #5695 ) ;
#12761 = EDGE_CURVE ( 'NONE', #5214, #1970, #7926, .T. ) ;
#12762 = CARTESIAN_POINT ( 'NONE',  ( -239.5361044668155159, 1.848645179572584896, 11.60366368868220022 ) ) ;
#12763 = SHAPE_REPRESENTATION_RELATIONSHIP ( 'NONE' , 'NONE' ,  #4340, #3952 ) ;
#12764 = CARTESIAN_POINT ( 'NONE',  ( 0.000000000000000000, 30.00000000000000000, 208.0000000000000000 ) ) ;
#12765 = CIRCLE ( 'NONE', #8093, 4.500000000000000000 ) ;
#12766 = ORIENTED_EDGE ( 'NONE', *, *, #8600, .F. ) ;
#12767 = DIRECTION ( 'NONE',  ( 0.6368676505102707219, 0.000000000000000000, 0.7709731485165535192 ) ) ;
#12768 = ORIENTED_EDGE ( 'NONE', *, *, #10700, .T. ) ;
#12769 = DIRECTION ( 'NONE',  ( 0.000000000000000000, 0.000000000000000000, 1.000000000000000000 ) ) ;
#12770 = ORIENTED_EDGE ( 'NONE', *, *, #278, .F. ) ;
#12771 = VECTOR ( 'NONE', #5404, 1000.000000000000227 ) ;
#12772 = CARTESIAN_POINT ( 'NONE',  ( 239.9543636722321764, -1.989473563294940961, -2.884354563557201434 ) ) ;
#12773 = DIRECTION ( 'NONE',  ( -0.000000000000000000, -1.000000000000000000, 0.000000000000000000 ) ) ;
#12774 = CARTESIAN_POINT ( 'NONE',  ( -249.7800409167773807, -11.57739048714482522, 3.170426907214261458 ) ) ;
#12775 = DIRECTION ( 'NONE',  ( 0.000000000000000000, 1.000000000000000000, 0.000000000000000000 ) ) ;
#12776 = CONICAL_SURFACE ( 'NONE', #3200, 6.500000000000005329, 0.7853981633974490562 ) ;
#12777 = LINE ( 'NONE', #3640, #12184 ) ;
#12778 = CARTESIAN_POINT ( 'NONE',  ( 0.000000000000000000, 19.00000000000000000, 208.0000000000000000 ) ) ;
#12779 = DIRECTION ( 'NONE',  ( 0.6368676505102709440, 0.000000000000000000, 0.7709731485165532971 ) ) ;
#12780 = ITEM_DEFINED_TRANSFORMATION ( 'NONE', 'NONE', #1296,  #805 ) ;
#12782 = ORIENTED_EDGE ( 'NONE', *, *, #9125, .T. ) ;
#12781 = AXIS2_PLACEMENT_3D ( 'NONE', #2514, #9646, #6596 ) ;
#12783 = ORIENTED_EDGE ( 'NONE', *, *, #10460, .T. ) ;
#12784 = CARTESIAN_POINT ( 'NONE',  ( -249.7982158286841639, -11.73176039257149661, 0.7224695965638833206 ) ) ;
#12785 = VERTEX_POINT ( 'NONE', #5931 ) ;
#12786 = CARTESIAN_POINT ( 'NONE',  ( -84.14846197958475216, 19.96883746048893471, -247.8175805193368717 ) ) ;
#12787 = DIRECTION ( 'NONE',  ( 1.000000000000000000, 0.000000000000000000, 0.000000000000000000 ) ) ;
#12788 = DIRECTION ( 'NONE',  ( 0.000000000000000000, 0.7071067811865450192, 0.7071067811865500152 ) ) ;
#12789 = LINE ( 'NONE', #12531, #1284 ) ;
#12790 = CARTESIAN_POINT ( 'NONE',  ( -171.8850263962758902, 20.08915143297736705, 196.0019244007916370 ) ) ;
#12791 = EDGE_CURVE ( 'NONE', #4005, #2425, #12700, .T. ) ;
#12792 = LINE ( 'NONE', #800, #1443 ) ;
#12793 = EDGE_CURVE ( 'NONE', #3319, #11817, #6126, .T. ) ;
#12794 = LINE ( 'NONE', #12602, #13024 ) ;
#12795 = CARTESIAN_POINT ( 'NONE',  ( 3.647576077975348330, -138.4705547276867321, -41.69198534955602042 ) ) ;
#12796 = CARTESIAN_POINT ( 'NONE',  ( -229.7194722698235125, -3.038862843935012936, -11.35678684944393346 ) ) ;
#12797 = AXIS2_PLACEMENT_3D ( 'NONE', #1909, #6720, #4627 ) ;
#12798 = CARTESIAN_POINT ( 'NONE',  ( -249.2754563888320547, 10.50954084450174975, -5.254718384040748091 ) ) ;
#12799 = CARTESIAN_POINT ( 'NONE',  ( 23.54981712579821362, -30.00000000000000000, -295.6955080056602583 ) ) ;
#12800 = CARTESIAN_POINT ( 'NONE',  ( 0.000000000000000000, 22.00000000000000000, 0.000000000000000000 ) ) ;
#12801 =( REPRESENTATION_RELATIONSHIP ('NONE','NONE', #12019, #182 ) REPRESENTATION_RELATIONSHIP_WITH_TRANSFORMATION ( #122 )SHAPE_REPRESENTATION_RELATIONSHIP( ) );
#12802 = DIRECTION ( 'NONE',  ( -0.000000000000000000, -1.000000000000000000, 0.000000000000000000 ) ) ;
#12803 = ORIENTED_EDGE ( 'NONE', *, *, #12741, .F. ) ;
#12804 = ORIENTED_EDGE ( 'NONE', *, *, #6795, .T. ) ;
#12805 = PRODUCT_RELATED_PRODUCT_CATEGORY ( 'part', '', ( #3805 ) ) ;
#12806 = CARTESIAN_POINT ( 'NONE',  ( -5.000000000000000000, 0.000000000000000000, 250.0000000000000000 ) ) ;
#12807 = FACE_OUTER_BOUND ( 'NONE', #10654, .T. ) ;
#12808 = CARTESIAN_POINT ( 'NONE',  ( 252.9796497720277841, 20.55460285096646089, 67.76049180220992696 ) ) ;
#12809 = CARTESIAN_POINT ( 'NONE',  ( 0.000000000000000000, 9.830508068699479907, 0.000000000000000000 ) ) ;
#12810 = CARTESIAN_POINT ( 'NONE',  ( 0.000000000000000000, 0.000000000000000000, 0.000000000000000000 ) ) ;
#12811 = LINE ( 'NONE', #1554, #11792 ) ;
#12812 = DIRECTION ( 'NONE',  ( -1.000000000000000000, 0.000000000000000000, 0.000000000000000000 ) ) ;
#12813 = ORIENTED_EDGE ( 'NONE', *, *, #5209, .T. ) ;
#12814 = CARTESIAN_POINT ( 'NONE',  ( -0.000000000000000000, -22.00000000000000000, 0.000000000000000000 ) ) ;
#12815 = EDGE_LOOP ( 'NONE', ( #6792, #2874, #8700, #9944, #5489, #11524 ) ) ;
#12816 = ORIENTED_EDGE ( 'NONE', *, *, #9319, .F. ) ;
#12817 = ADVANCED_FACE ( 'NONE', ( #7522 ), #4570, .F. ) ;
#12818 = CIRCLE ( 'NONE', #8993, 5.100000000000003197 ) ;
#12819 = ADVANCED_FACE ( 'NONE', ( #331 ), #9942, .F. ) ;
#12820 = CARTESIAN_POINT ( 'NONE',  ( 115.3046144132251385, 20.08915143297736350, 233.8077470125392665 ) ) ;
#12821 = ORIENTED_EDGE ( 'NONE', *, *, #5302, .T. ) ;
#12822 = PRODUCT_DEFINITION_SHAPE ( 'NONE', 'NONE',  #13101 ) ;
#12823 = CIRCLE ( 'NONE', #1971, 5.499999999999998224 ) ;
#12824 = CARTESIAN_POINT ( 'NONE',  ( -197.8197553893924976, 30.00000000000000000, -64.27553482998719403 ) ) ;
#12825 = DIRECTION ( 'NONE',  ( 0.000000000000000000, 1.000000000000000000, 0.000000000000000000 ) ) ;
#12826 = AXIS2_PLACEMENT_3D ( 'NONE', #7208, #2927, #7013 ) ;
#12827 = CARTESIAN_POINT ( 'NONE',  ( 158.9353507265259964, 20.08915143275230974, -207.1687172319319927 ) ) ;
#12828 = DIRECTION ( 'NONE',  ( 0.000000000000000000, -1.000000000000000000, 0.000000000000000000 ) ) ;
#12829 = DIRECTION ( 'NONE',  ( 0.6368676505102689456, 0.000000000000000000, 0.7709731485165549625 ) ) ;
#12830 =( REPRESENTATION_RELATIONSHIP ('NONE','NONE', #12019, #5191 ) REPRESENTATION_RELATIONSHIP_WITH_TRANSFORMATION ( #12334 )SHAPE_REPRESENTATION_RELATIONSHIP( ) );
#12831 = EDGE_LOOP ( 'NONE', ( #11177, #3347, #7770, #9467 ) ) ;
#12832 = CARTESIAN_POINT ( 'NONE',  ( -27.68945685411286561, -19.00000000000000000, 290.6841825403027997 ) ) ;
#12833 = CONICAL_SURFACE ( 'NONE', #917, 6.500000000000005329, 0.7853981633974518317 ) ;
#12834 = ORIENTED_EDGE ( 'NONE', *, *, #11893, .F. ) ;
#12835 = AXIS2_PLACEMENT_3D ( 'NONE', #12960, #5839, #10896 ) ;
#12836 = CARTESIAN_POINT ( 'NONE',  ( -243.1363860134830759, 7.429686608631851819, -9.102873391464031627 ) ) ;
#12837 = EDGE_LOOP ( 'NONE', ( #4113, #4495, #11941, #9727 ) ) ;
#12838 = EDGE_CURVE ( 'NONE', #3738, #3634, #1013, .T. ) ;
#12839 = CARTESIAN_POINT ( 'NONE',  ( 240.2635760545757933, -2.467011615924421974, -2.483268943700265741 ) ) ;
#12840 = CARTESIAN_POINT ( 'NONE',  ( 0.000000000000000000, 0.000000000000000000, 0.000000000000000000 ) ) ;
#12841 = DIRECTION ( 'NONE',  ( -0.4503334343941441942, 0.7071067811865670016, -0.5451603414287832239 ) ) ;
#12842 = AXIS2_PLACEMENT_3D ( 'NONE', #2557, #3690, #701 ) ;
#12843 = DIRECTION ( 'NONE',  ( 0.000000000000000000, -1.000000000000000000, 0.000000000000000000 ) ) ;
#12844 = AXIS2_PLACEMENT_3D ( 'NONE', #3103, #2303, #8454 ) ;
#12845 = EDGE_CURVE ( 'NONE', #5922, #2972, #2385, .T. ) ;
#12846 = CARTESIAN_POINT ( 'NONE',  ( -241.3346421314001020, -5.383590977517163978, 10.72461093951733169 ) ) ;
#12847 = CARTESIAN_POINT ( 'NONE',  ( 225.1241593668336236, -18.00000000000000000, -185.9653539489990521 ) ) ;
#12848 = VERTEX_POINT ( 'NONE', #1390 ) ;
#12849 = CARTESIAN_POINT ( 'NONE',  ( -229.9857278087561951, 11.72347515457171419, 2.588372091913021755 ) ) ;
#12850 = CONTEXT_DEPENDENT_SHAPE_REPRESENTATION ( #8605, #8558 ) ;
#12851 = EDGE_LOOP ( 'NONE', ( #11703, #5361, #12285, #3699 ) ) ;
#12852 = PRODUCT_DEFINITION_SHAPE ( 'NONE', 'NONE',  #13075 ) ;
#12853 = CIRCLE ( 'NONE', #10517, 230.0000000000000000 ) ;
#12854 = VERTEX_POINT ( 'NONE', #5517 ) ;
#12855 = CARTESIAN_POINT ( 'NONE',  ( -248.5304950467331082, -9.965644880995725430, -6.224989825265568655 ) ) ;
#12856 = ORIENTED_EDGE ( 'NONE', *, *, #9152, .T. ) ;
#12857 = CARTESIAN_POINT ( 'NONE',  ( -226.7975291074607469, 20.55460285152577526, 130.9697226057901673 ) ) ;
#12858 = CARTESIAN_POINT ( 'NONE',  ( -0.000000000000000000, -25.50000000000000000, 0.000000000000000000 ) ) ;
#12859 = LINE ( 'NONE', #6738, #8924 ) ;
#12860 = DIRECTION ( 'NONE',  ( 0.5469441386039890496, 0.000000000000000000, -0.8371691043312220470 ) ) ;
#12861 = CARTESIAN_POINT ( 'NONE',  ( 3.059167704270088292E-14, 29.00000000000000000, 249.7999999999999829 ) ) ;
#12862 = CIRCLE ( 'NONE', #1166, 6.500000000000005329 ) ;
#12863 = CARTESIAN_POINT ( 'NONE',  ( 135.8846079354933352, -30.00000000000000000, -256.1940150085812888 ) ) ;
#12864 = CARTESIAN_POINT ( 'NONE',  ( 14.31396777367097251, -138.4705547276867321, -39.32730324096123553 ) ) ;
#12865 = AXIS2_PLACEMENT_3D ( 'NONE', #1863, #11120, #12123 ) ;
#12866 = CARTESIAN_POINT ( 'NONE',  ( -229.8303177822455439, -7.754159524086684740, -8.836599804383647339 ) ) ;
#12867 =( BOUNDED_CURVE ( )  B_SPLINE_CURVE ( 3, ( #5474, #8672, #9532, #4400 ),
 .UNSPECIFIED., .F., .F. ) 
 B_SPLINE_CURVE_WITH_KNOTS ( ( 4, 4 ),
 ( 0.000000000000000000, 1.000000000000000000 ),
 .UNSPECIFIED. ) 
 CURVE ( )  GEOMETRIC_REPRESENTATION_ITEM ( )  RATIONAL_B_SPLINE_CURVE ( ( 1.000000000000000000, 0.4027746460044325238, 0.4027746460044325238, 1.000000000000000000 ) ) 
 REPRESENTATION_ITEM ( '' )  );
#12868 = CARTESIAN_POINT ( 'NONE',  ( -249.7928741345566834, 11.67611540995070207, -1.322401136026368107 ) ) ;
#12869 = CARTESIAN_POINT ( 'NONE',  ( -241.5877467159411083, -5.754636831476545922, -10.53299718410284314 ) ) ;
#12870 = CARTESIAN_POINT ( 'NONE',  ( -229.7631934145547632, -5.935281959122680639, -10.43610481315899996 ) ) ;
#12871 = EDGE_LOOP ( 'NONE', ( #2647, #5944, #12137, #2364 ) ) ;
#12872 = ORIENTED_EDGE ( 'NONE', *, *, #1101, .T. ) ;
#12873 = EDGE_CURVE ( 'NONE', #4498, #6924, #12078, .T. ) ;
#12874 = AXIS2_PLACEMENT_3D ( 'NONE', #4860, #12064, #10126 ) ;
#12875 = LINE ( 'NONE', #8947, #8215 ) ;
#12876 = FACE_BOUND ( 'NONE', #9780, .T. ) ;
#12877 = CARTESIAN_POINT ( 'NONE',  ( -34.13493237021134519, 20.79694577641179620, -259.0935598599534728 ) ) ;
#12878 = FACE_OUTER_BOUND ( 'NONE', #5946, .T. ) ;
#12879 = CARTESIAN_POINT ( 'NONE',  ( 0.000000000000000000, 0.000000000000000000, 0.000000000000000000 ) ) ;
#12880 = FACE_OUTER_BOUND ( 'NONE', #339, .T. ) ;
#12881 = DIRECTION ( 'NONE',  ( -0.4503334343941556295, 0.7071067811865489050, -0.5451603414287969906 ) ) ;
#12882 = AXIS2_PLACEMENT_3D ( 'NONE', #3858, #4927, #5125 ) ;
#12883 =( REPRESENTATION_RELATIONSHIP ('NONE','NONE', #12019, #5191 ) REPRESENTATION_RELATIONSHIP_WITH_TRANSFORMATION ( #3795 )SHAPE_REPRESENTATION_RELATIONSHIP( ) );
#12884 = ORIENTED_EDGE ( 'NONE', *, *, #5677, .F. ) ;
#12885 = FACE_OUTER_BOUND ( 'NONE', #6026, .T. ) ;
#12886 = VERTEX_POINT ( 'NONE', #11457 ) ;
#12887 = VERTEX_POINT ( 'NONE', #9640 ) ;
#12888 = EDGE_CURVE ( 'NONE', #2076, #366, #11229, .T. ) ;
#12889 = CARTESIAN_POINT ( 'NONE',  ( -7.780566028168587395E-13, 20.08915143297736350, 260.5542428351130866 ) ) ;
#12890 = VERTEX_POINT ( 'NONE', #5392 ) ;
#12891 = AXIS2_PLACEMENT_3D ( 'NONE', #2802, #8681, #5685 ) ;
#12892 = LINE ( 'NONE', #1696, #5603 ) ;
#12893 = CARTESIAN_POINT ( 'NONE',  ( 239.0510843050431617, -0.6173067666910034834, -3.446156762516083383 ) ) ;
#12894 = CARTESIAN_POINT ( 'NONE',  ( -17.05314194195814892, 20.08915143288246696, 260.5542428355875018 ) ) ;
#12895 = LINE ( 'NONE', #11838, #5623 ) ;
#12896 =( LENGTH_UNIT ( ) NAMED_UNIT ( * ) SI_UNIT ( .MILLI., .METRE. ) );
#12897 = CARTESIAN_POINT ( 'NONE',  ( 290.6841825403032544, -29.00000000000000000, 27.68945685411186730 ) ) ;
#12898 = EDGE_CURVE ( 'NONE', #4565, #1001, #2847, .T. ) ;
#12899 = ADVANCED_FACE ( 'NONE', ( #5913 ), #6338, .F. ) ;
#12900 = ORIENTED_EDGE ( 'NONE', *, *, #10673, .T. ) ;
#12901 = LINE ( 'NONE', #2376, #9650 ) ;
#12902 = EDGE_LOOP ( 'NONE', ( #11453, #7958, #1287, #3715 ) ) ;
#12903 = CARTESIAN_POINT ( 'NONE',  ( -246.5915682062262988, 9.436693423219887578, -7.000847393187709322 ) ) ;
#12904 = ORIENTED_EDGE ( 'NONE', *, *, #3195, .T. ) ;
#12905 = DIRECTION ( 'NONE',  ( 1.224646799147349509E-16, 0.000000000000000000, -1.000000000000000000 ) ) ;
#12906 = DIRECTION ( 'NONE',  ( 0.6368676505102695007, 0.000000000000000000, 0.7709731485165545184 ) ) ;
#12907 = LINE ( 'NONE', #3637, #7438 ) ;
#12908 = CARTESIAN_POINT ( 'NONE',  ( -229.7036030501511732, 1.544435828463907923, -11.67381294332149011 ) ) ;
#12909 = CARTESIAN_POINT ( 'NONE',  ( -253.8843055347120412, 20.08915143297736705, 59.19439222780385279 ) ) ;
#12910 = CARTESIAN_POINT ( 'NONE',  ( -244.6143483479685869, -8.518413533159836959, 8.452629830878873207 ) ) ;
#12911 = EDGE_CURVE ( 'NONE', #468, #12676, #3131, .T. ) ;
#12912 = CARTESIAN_POINT ( 'NONE',  ( -17.06764083276443955, 20.79694577634646890, -260.3553053170167004 ) ) ;
#12913 = ORIENTED_EDGE ( 'NONE', *, *, #9890, .T. ) ;
#12914 = CARTESIAN_POINT ( 'NONE',  ( -233.0000000000000000, -1.000000000000000000, -12.50000000000000000 ) ) ;
#12915 = ORIENTED_EDGE ( 'NONE', *, *, #6502, .T. ) ;
#12916 = EDGE_CURVE ( 'NONE', #4958, #678, #3838, .T. ) ;
#12917 = ORIENTED_EDGE ( 'NONE', *, *, #9709, .F. ) ;
#12918 = AXIS2_PLACEMENT_3D ( 'NONE', #5281, #4282, #2220 ) ;
#12919 = CARTESIAN_POINT ( 'NONE',  ( -249.0998459883950318, -10.33180199792140819, -5.596503888595450782 ) ) ;
#12920 = EDGE_LOOP ( 'NONE', ( #6422, #9448, #6813, #4612 ) ) ;
#12921 = CARTESIAN_POINT ( 'NONE',  ( 172.6991790967991847, 20.55460285078499183, -196.8887528227133714 ) ) ;
#12922 = DIRECTION ( 'NONE',  ( 0.000000000000000000, 0.9998057603070481525, -0.01970892327970900221 ) ) ;
#12923 = FACE_OUTER_BOUND ( 'NONE', #12034, .T. ) ;
#12924 = CARTESIAN_POINT ( 'NONE',  ( 3.012631125902489062E-14, 24.99999999999995737, 246.0000000000000000 ) ) ;
#12925 = DIRECTION ( 'NONE',  ( -0.000000000000000000, -1.000000000000000000, 0.000000000000000000 ) ) ;
#12926 = CARTESIAN_POINT ( 'NONE',  ( 0.000000000000000000, 0.000000000000000000, 0.000000000000000000 ) ) ;
#12927 = DIRECTION ( 'NONE',  ( -0.3518698652246342595, 0.5538822189107472926, -0.7545873610930050601 ) ) ;
#12928 = CARTESIAN_POINT ( 'NONE',  ( 229.9785170508817487, 1.553259044379982301, 3.144732723172867672 ) ) ;
#12929 = ITEM_DEFINED_TRANSFORMATION ( 'NONE', 'NONE', #12364,  #805 ) ;
#12930 = PRODUCT_DEFINITION_SHAPE ( 'NONE', 'NONE',  #13130 ) ;
#12931 = CARTESIAN_POINT ( 'NONE',  ( -249.7367190369228069, 11.37209550732486640, -2.959943707653969636 ) ) ;
#12932 = CARTESIAN_POINT ( 'NONE',  ( -246.7640704946416861, -9.498771479503499648, -7.332983348641192833 ) ) ;
#12933 = CIRCLE ( 'NONE', #7191, 2.000000000000000444 ) ;
#12934 = CARTESIAN_POINT ( 'NONE',  ( -229.9651640739562879, -11.31348253173457152, -4.017925228533020032 ) ) ;
#12935 = VERTEX_POINT ( 'NONE', #5852 ) ;
#12936 = ORIENTED_EDGE ( 'NONE', *, *, #12587, .F. ) ;
#12937 = FACE_OUTER_BOUND ( 'NONE', #10442, .T. ) ;
#12938 = DIRECTION ( 'NONE',  ( 0.000000000000000000, 0.000000000000000000, 1.000000000000000000 ) ) ;
#12939 = CARTESIAN_POINT ( 'NONE',  ( 226.7975291075301811, 20.55460285098495277, 130.9697226058104036 ) ) ;
#12940 = DIRECTION ( 'NONE',  ( 1.000000000000000000, 0.000000000000000000, 0.000000000000000000 ) ) ;
#12941 = DIRECTION ( 'NONE',  ( 0.9961946980917465444, 0.000000000000000000, -0.08715574274764853469 ) ) ;
#12942 = DIRECTION ( 'NONE',  ( 0.000000000000000000, 1.000000000000000000, 0.000000000000000000 ) ) ;
#12943 = CARTESIAN_POINT ( 'NONE',  ( 240.1157413331974908, 2.212437690464817308, -2.712157915439629363 ) ) ;
#12944 = ADVANCED_FACE ( 'NONE', ( #10777 ), #6549, .F. ) ;
#12945 = ORIENTED_EDGE ( 'NONE', *, *, #10215, .F. ) ;
#12946 = AXIS2_PLACEMENT_3D ( 'NONE', #9090, #8095, #3010 ) ;
#12947 = LINE ( 'NONE', #1886, #7428 ) ;
#12948 = VERTEX_POINT ( 'NONE', #4631 ) ;
#12949 = CIRCLE ( 'NONE', #7206, 239.0000000000000000 ) ;
#12950 = ORIENTED_EDGE ( 'NONE', *, *, #2602, .F. ) ;
#12951 = AXIS2_PLACEMENT_3D ( 'NONE', #3935, #8873, #12140 ) ;
#12952 = CIRCLE ( 'NONE', #1458, 240.3921568627449687 ) ;
#12953 = AXIS2_PLACEMENT_3D ( 'NONE', #5205, #87, #11280 ) ;
#12954 = CARTESIAN_POINT ( 'NONE',  ( 240.0731061099998271, -2.151402440700775909, 2.761193928001421050 ) ) ;
#12955 = EDGE_LOOP ( 'NONE', ( #11875, #10740, #7431, #5228 ) ) ;
#12956 = TOROIDAL_SURFACE ( 'NONE', #3584, 250.0000000000000000, 10.00000000000000000 ) ;
#12957 = CARTESIAN_POINT ( 'NONE',  ( -240.1208361041834962, -2.772967769359314882, 11.41810622433041900 ) ) ;
#12958 = CARTESIAN_POINT ( 'NONE',  ( -196.2980642837470100, 20.08915143287812199, -172.1812796682245050 ) ) ;
#12959 = CARTESIAN_POINT ( 'NONE',  ( -0.000000000000000000, -25.00000000000000000, 0.000000000000000000 ) ) ;
#12960 = CARTESIAN_POINT ( 'NONE',  ( -249.7999999999999829, -20.00000000000000000, 0.000000000000000000 ) ) ;
#12961 = EDGE_CURVE ( 'NONE', #10559, #10688, #4057, .T. ) ;
#12962 = ADVANCED_FACE ( 'NONE', ( #782 ), #7396, .F. ) ;
#12963 = PRODUCT_DEFINITION_SHAPE ( 'NONE', 'NONE',  #13079 ) ;
#12964 = AXIS2_PLACEMENT_3D ( 'NONE', #3784, #11092, #9785 ) ;
#12965 = ORIENTED_EDGE ( 'NONE', *, *, #1973, .F. ) ;
#12966 = DIRECTION ( 'NONE',  ( 0.000000000000000000, 1.000000000000000000, 0.000000000000000000 ) ) ;
#12967 = AXIS2_PLACEMENT_3D ( 'NONE', #6355, #8426, #3139 ) ;
#12968 = ORIENTED_EDGE ( 'NONE', *, *, #3356, .F. ) ;
#12969 = CARTESIAN_POINT ( 'NONE',  ( 239.1818646735695211, 0.9924701939458496769, 3.356351167333999630 ) ) ;
#12970 = DIRECTION ( 'NONE',  ( 0.000000000000000000, 0.000000000000000000, 1.000000000000000000 ) ) ;
#12971 = ORIENTED_EDGE ( 'NONE', *, *, #9641, .F. ) ;
#12972 = VECTOR ( 'NONE', #662, 1000.000000000000000 ) ;
#12973 = ADVANCED_FACE ( 'NONE', ( #4701, #2695 ), #6785, .F. ) ;
#12974 = AXIS2_PLACEMENT_3D ( 'NONE', #10567, #2293, #12441 ) ;
#12975 = DIRECTION ( 'NONE',  ( 0.000000000000000000, 0.9998057603070480415, -0.01970892327970899874 ) ) ;
#12976 = DIRECTION ( 'NONE',  ( 0.000000000000000000, 1.000000000000000000, 0.000000000000000000 ) ) ;
#12977 = CARTESIAN_POINT ( 'NONE',  ( -7.780566028168587395E-13, 20.08915143297736350, 260.5542428351130866 ) ) ;
#12978 = CARTESIAN_POINT ( 'NONE',  ( -241.3126941818472631, -5.350247869156489422, 10.74127079069803514 ) ) ;
#12979 = CARTESIAN_POINT ( 'NONE',  ( -239.6569666423348792, 1.960938215982088728, -11.83870082074197860 ) ) ;
#12980 = ITEM_DEFINED_TRANSFORMATION ( 'NONE', 'NONE', #4420,  #805 ) ;
#12981 =( REPRESENTATION_RELATIONSHIP ('NONE','NONE', #12019, #182 ) REPRESENTATION_RELATIONSHIP_WITH_TRANSFORMATION ( #2699 )SHAPE_REPRESENTATION_RELATIONSHIP( ) );
#12982 = ORIENTED_EDGE ( 'NONE', *, *, #8350, .T. ) ;
#12983 = CARTESIAN_POINT ( 'NONE',  ( -238.7112179666109739, -0.03612072660172950533, -11.74994901723889384 ) ) ;
#12984 = TOROIDAL_SURFACE ( 'NONE', #7020, 250.7029414592220178, 3.000000000000000000 ) ;
#12985 = VERTEX_POINT ( 'NONE', #8911 ) ;
#12986 = EDGE_LOOP ( 'NONE', ( #10890, #2523, #7912, #2065, #10143, #8827, #12370, #8389 ) ) ;
#12987 = DIRECTION ( 'NONE',  ( 0.6368676505102707219, 0.000000000000000000, 0.7709731485165535192 ) ) ;
#12988 = ORIENTED_EDGE ( 'NONE', *, *, #2752, .F. ) ;
#12989 = ADVANCED_FACE ( 'NONE', ( #6919 ), #1849, .T. ) ;
#12990 = CARTESIAN_POINT ( 'NONE',  ( -247.9906035367588402, 20.55460285060343040, -84.20717312374212327 ) ) ;
#12991 = EDGE_CURVE ( 'NONE', #9366, #2361, #9102, .T. ) ;
#12992 = CARTESIAN_POINT ( 'NONE',  ( 0.000000000000000000, 19.00000000000000000, 0.000000000000000000 ) ) ;
#12993 = FACE_OUTER_BOUND ( 'NONE', #1509, .T. ) ;
#12994 = DIRECTION ( 'NONE',  ( 0.000000000000000000, 0.9998057603070481525, -0.01970892327970899874 ) ) ;
#12995 = CARTESIAN_POINT ( 'NONE',  ( -240.5991998575718185, 4.074980142617108392, 11.29000474999590331 ) ) ;
#12996 =( REPRESENTATION_RELATIONSHIP ('NONE','NONE', #12019, #182 ) REPRESENTATION_RELATIONSHIP_WITH_TRANSFORMATION ( #10080 )SHAPE_REPRESENTATION_RELATIONSHIP( ) );
#12997 = AXIS2_PLACEMENT_3D ( 'NONE', #11811, #10795, #12006 ) ;
#12998 = DIRECTION ( 'NONE',  ( 0.000000000000000000, 0.000000000000000000, 1.000000000000000000 ) ) ;
#12999 = DIRECTION ( 'NONE',  ( -0.6378047977532502744, 0.5538822189107472926, -0.5351817705578573170 ) ) ;
#13000 = DIRECTION ( 'NONE',  ( 0.6368676505102689456, 0.000000000000000000, 0.7709731485165549625 ) ) ;
#13001 = APPLICATION_CONTEXT ( 'automotive_design' ) ;
#13002 = CARTESIAN_POINT ( 'NONE',  ( -249.7849245721639591, 11.61140107782044240, -1.799432315875151733 ) ) ;
#13003 = CARTESIAN_POINT ( 'NONE',  ( 71.82423009839129691, 19.40000000000000213, -197.3354503650404865 ) ) ;
#13004 = ORIENTED_EDGE ( 'NONE', *, *, #7193, .T. ) ;
#13005 = ORIENTED_EDGE ( 'NONE', *, *, #2878, .T. ) ;
#13006 = PRODUCT_DEFINITION_FORMATION_WITH_SPECIFIED_SOURCE ( 'ANY', '', #439, .NOT_KNOWN. ) ;
#13007 = DIRECTION ( 'NONE',  ( -0.000000000000000000, -1.000000000000000000, 0.000000000000000000 ) ) ;
#13008 = ADVANCED_FACE ( 'NONE', ( #1804 ), #10157, .F. ) ;
#13009 = FACE_OUTER_BOUND ( 'NONE', #415, .T. ) ;
#13010 = CARTESIAN_POINT ( 'NONE',  ( 67.61424743001118998, 20.79694577617620155, -252.4341100437179648 ) ) ;
#13011 = DIRECTION ( 'NONE',  ( 0.000000000000000000, 1.000000000000000000, 0.000000000000000000 ) ) ;
#13012 = CARTESIAN_POINT ( 'NONE',  ( 0.000000000000000000, 0.000000000000000000, 0.000000000000000000 ) ) ;
#13013 = CARTESIAN_POINT ( 'NONE',  ( -245.3661487643706209, -8.922833484614967503, 7.644980496220819433 ) ) ;
#13014 = COLOUR_RGB ( '', 0.66274510, 0.83137255, 0.94901961) ;
#13015 = CARTESIAN_POINT ( 'NONE',  ( 11.00000000000000000, 0.000000000000000000, 240.0999999999999943 ) ) ;
#13016 = VERTEX_POINT ( 'NONE', #9927 ) ;
#13017 = FACE_BOUND ( 'NONE', #3646, .T. ) ;
#13018 = CARTESIAN_POINT ( 'NONE',  ( -239.3393815604536883, -1.669038146043678950, 11.88372659485297689 ) ) ;
#13019 = ORIENTED_EDGE ( 'NONE', *, *, #1030, .T. ) ;
#13020 = ORIENTED_EDGE ( 'NONE', *, *, #1466, .T. ) ;
#13021 = LINE ( 'NONE', #767, #5296 ) ;
#13022 = ORIENTED_EDGE ( 'NONE', *, *, #3747, .T. ) ;
#13023 = FACE_OUTER_BOUND ( 'NONE', #12098, .T. ) ;
#13024 = VECTOR ( 'NONE', #3658, 1000.000000000000000 ) ;
#13025 = CARTESIAN_POINT ( 'NONE',  ( -252.2208631662124958, 20.08915143301432948, -67.55708173888800161 ) ) ;
#13026 = CARTESIAN_POINT ( 'NONE',  ( -238.7054577244453242, -0.2141779405393015034, -11.99854502521326793 ) ) ;
#13027 =( NAMED_UNIT ( * ) SI_UNIT ( $, .STERADIAN. ) SOLID_ANGLE_UNIT ( ) );
#13028 = ORIENTED_EDGE ( 'NONE', *, *, #6091, .T. ) ;
#13029 = CARTESIAN_POINT ( 'NONE',  ( 233.5975020798683204, -2.199572672675505824, 0.04335963121536006576 ) ) ;
#13030 = AXIS2_PLACEMENT_3D ( 'NONE', #5672, #4533, #2472 ) ;
#13031 = VERTEX_POINT ( 'NONE', #12003 ) ;
#13032 = CARTESIAN_POINT ( 'NONE',  ( 0.000000000000000000, -19.00000000000000000, 0.000000000000000000 ) ) ;
#13033 = VERTEX_POINT ( 'NONE', #12861 ) ;
#13034 = ADVANCED_BREP_SHAPE_REPRESENTATION ( '', ( #1548, #805 ), #9955 ) ;
#13035 = AXIS2_PLACEMENT_3D ( 'NONE', #5819, #8877, #7677 ) ;
#13036 = TOROIDAL_SURFACE ( 'NONE', #3667, 250.0000000000000000, 10.00000000000000000 ) ;
#13037 = EDGE_CURVE ( 'NONE', #3121, #10050, #12402, .T. ) ;
#13038 = EDGE_CURVE ( 'NONE', #9134, #5226, #5801, .T. ) ;
#13039 = CARTESIAN_POINT ( 'NONE',  ( 240.0821326533886975, -2.149019271346159776, -2.771577408434056533 ) ) ;
#13040 = CARTESIAN_POINT ( 'NONE',  ( -241.3883989931630083, -5.445712471323459702, -10.41186067205816812 ) ) ;
#13041 = NEXT_ASSEMBLY_USAGE_OCCURRENCE ( 'NAUO1', ' ', ' ', #6540, #7672, $ ) ;
#13042 = NEXT_ASSEMBLY_USAGE_OCCURRENCE ( 'NAUO2', ' ', ' ', #6540, #11012, $ ) ;
#13043 = NEXT_ASSEMBLY_USAGE_OCCURRENCE ( 'NAUO3', ' ', ' ', #6540, #2767, $ ) ;
#13044 = NEXT_ASSEMBLY_USAGE_OCCURRENCE ( 'NAUO4', ' ', ' ', #6540, #9065, $ ) ;
#13045 = NEXT_ASSEMBLY_USAGE_OCCURRENCE ( 'NAUO5', ' ', ' ', #6540, #8087, $ ) ;
#13046 = NEXT_ASSEMBLY_USAGE_OCCURRENCE ( 'NAUO6', ' ', ' ', #6540, #5139, $ ) ;
#13047 = NEXT_ASSEMBLY_USAGE_OCCURRENCE ( 'NAUO7', ' ', ' ', #6540, #10447, $ ) ;
#13048 = NEXT_ASSEMBLY_USAGE_OCCURRENCE ( 'NAUO8', ' ', ' ', #6540, #12069, $ ) ;
#13049 = NEXT_ASSEMBLY_USAGE_OCCURRENCE ( 'NAUO9', ' ', ' ', #6540, #12069, $ ) ;
#13050 = NEXT_ASSEMBLY_USAGE_OCCURRENCE ( 'NAUO10', ' ', ' ', #6540, #12069, $ ) ;
#13051 = NEXT_ASSEMBLY_USAGE_OCCURRENCE ( 'NAUO11', ' ', ' ', #6540, #12069, $ ) ;
#13052 = NEXT_ASSEMBLY_USAGE_OCCURRENCE ( 'NAUO12', ' ', ' ', #6540, #12069, $ ) ;
#13053 = NEXT_ASSEMBLY_USAGE_OCCURRENCE ( 'NAUO13', ' ', ' ', #6540, #12069, $ ) ;
#13054 = NEXT_ASSEMBLY_USAGE_OCCURRENCE ( 'NAUO14', ' ', ' ', #6540, #12069, $ ) ;
#13055 = NEXT_ASSEMBLY_USAGE_OCCURRENCE ( 'NAUO15', ' ', ' ', #6540, #12069, $ ) ;
#13056 = NEXT_ASSEMBLY_USAGE_OCCURRENCE ( 'NAUO16', ' ', ' ', #6540, #12069, $ ) ;
#13057 = NEXT_ASSEMBLY_USAGE_OCCURRENCE ( 'NAUO17', ' ', ' ', #6540, #12069, $ ) ;
#13058 = NEXT_ASSEMBLY_USAGE_OCCURRENCE ( 'NAUO18', ' ', ' ', #6540, #12069, $ ) ;
#13059 = NEXT_ASSEMBLY_USAGE_OCCURRENCE ( 'NAUO19', ' ', ' ', #6540, #12069, $ ) ;
#13060 = NEXT_ASSEMBLY_USAGE_OCCURRENCE ( 'NAUO20', ' ', ' ', #6540, #12069, $ ) ;
#13061 = NEXT_ASSEMBLY_USAGE_OCCURRENCE ( 'NAUO21', ' ', ' ', #6540, #12069, $ ) ;
#13062 = NEXT_ASSEMBLY_USAGE_OCCURRENCE ( 'NAUO22', ' ', ' ', #6540, #12069, $ ) ;
#13063 = NEXT_ASSEMBLY_USAGE_OCCURRENCE ( 'NAUO23', ' ', ' ', #6540, #12069, $ ) ;
#13064 = NEXT_ASSEMBLY_USAGE_OCCURRENCE ( 'NAUO24', ' ', ' ', #6540, #12069, $ ) ;
#13065 = NEXT_ASSEMBLY_USAGE_OCCURRENCE ( 'NAUO25', ' ', ' ', #6540, #12069, $ ) ;
#13066 = NEXT_ASSEMBLY_USAGE_OCCURRENCE ( 'NAUO26', ' ', ' ', #6540, #12069, $ ) ;
#13067 = NEXT_ASSEMBLY_USAGE_OCCURRENCE ( 'NAUO27', ' ', ' ', #6540, #12069, $ ) ;
#13068 = NEXT_ASSEMBLY_USAGE_OCCURRENCE ( 'NAUO28', ' ', ' ', #6540, #12069, $ ) ;
#13069 = NEXT_ASSEMBLY_USAGE_OCCURRENCE ( 'NAUO29', ' ', ' ', #6540, #12069, $ ) ;
#13070 = NEXT_ASSEMBLY_USAGE_OCCURRENCE ( 'NAUO30', ' ', ' ', #6540, #12069, $ ) ;
#13071 = NEXT_ASSEMBLY_USAGE_OCCURRENCE ( 'NAUO31', ' ', ' ', #6540, #12069, $ ) ;
#13072 = NEXT_ASSEMBLY_USAGE_OCCURRENCE ( 'NAUO32', ' ', ' ', #6540, #12069, $ ) ;
#13073 = NEXT_ASSEMBLY_USAGE_OCCURRENCE ( 'NAUO33', ' ', ' ', #6540, #12069, $ ) ;
#13074 = NEXT_ASSEMBLY_USAGE_OCCURRENCE ( 'NAUO34', ' ', ' ', #6540, #12069, $ ) ;
#13075 = NEXT_ASSEMBLY_USAGE_OCCURRENCE ( 'NAUO35', ' ', ' ', #6540, #12069, $ ) ;
#13076 = NEXT_ASSEMBLY_USAGE_OCCURRENCE ( 'NAUO36', ' ', ' ', #6540, #12069, $ ) ;
#13077 = NEXT_ASSEMBLY_USAGE_OCCURRENCE ( 'NAUO37', ' ', ' ', #6540, #12069, $ ) ;
#13078 = NEXT_ASSEMBLY_USAGE_OCCURRENCE ( 'NAUO38', ' ', ' ', #6540, #12069, $ ) ;
#13079 = NEXT_ASSEMBLY_USAGE_OCCURRENCE ( 'NAUO39', ' ', ' ', #6540, #12069, $ ) ;
#13080 = NEXT_ASSEMBLY_USAGE_OCCURRENCE ( 'NAUO40', ' ', ' ', #6540, #12069, $ ) ;
#13081 = NEXT_ASSEMBLY_USAGE_OCCURRENCE ( 'NAUO41', ' ', ' ', #6540, #12069, $ ) ;
#13082 = NEXT_ASSEMBLY_USAGE_OCCURRENCE ( 'NAUO42', ' ', ' ', #6540, #12069, $ ) ;
#13083 = NEXT_ASSEMBLY_USAGE_OCCURRENCE ( 'NAUO43', ' ', ' ', #6540, #12069, $ ) ;
#13084 = NEXT_ASSEMBLY_USAGE_OCCURRENCE ( 'NAUO44', ' ', ' ', #6540, #12069, $ ) ;
#13085 = NEXT_ASSEMBLY_USAGE_OCCURRENCE ( 'NAUO45', ' ', ' ', #6540, #12069, $ ) ;
#13086 = NEXT_ASSEMBLY_USAGE_OCCURRENCE ( 'NAUO46', ' ', ' ', #6540, #12069, $ ) ;
#13087 = NEXT_ASSEMBLY_USAGE_OCCURRENCE ( 'NAUO47', ' ', ' ', #6540, #12069, $ ) ;
#13088 = NEXT_ASSEMBLY_USAGE_OCCURRENCE ( 'NAUO48', ' ', ' ', #6540, #12069, $ ) ;
#13089 = NEXT_ASSEMBLY_USAGE_OCCURRENCE ( 'NAUO49', ' ', ' ', #6540, #12069, $ ) ;
#13090 = NEXT_ASSEMBLY_USAGE_OCCURRENCE ( 'NAUO50', ' ', ' ', #6540, #12069, $ ) ;
#13091 = NEXT_ASSEMBLY_USAGE_OCCURRENCE ( 'NAUO51', ' ', ' ', #6540, #12069, $ ) ;
#13092 = NEXT_ASSEMBLY_USAGE_OCCURRENCE ( 'NAUO52', ' ', ' ', #6540, #12069, $ ) ;
#13093 = NEXT_ASSEMBLY_USAGE_OCCURRENCE ( 'NAUO53', ' ', ' ', #6540, #12069, $ ) ;
#13094 = NEXT_ASSEMBLY_USAGE_OCCURRENCE ( 'NAUO54', ' ', ' ', #6540, #12069, $ ) ;
#13095 = NEXT_ASSEMBLY_USAGE_OCCURRENCE ( 'NAUO55', ' ', ' ', #6540, #12069, $ ) ;
#13096 = NEXT_ASSEMBLY_USAGE_OCCURRENCE ( 'NAUO56', ' ', ' ', #6540, #12069, $ ) ;
#13097 = NEXT_ASSEMBLY_USAGE_OCCURRENCE ( 'NAUO57', ' ', ' ', #6540, #12069, $ ) ;
#13098 = NEXT_ASSEMBLY_USAGE_OCCURRENCE ( 'NAUO58', ' ', ' ', #6540, #12069, $ ) ;
#13099 = NEXT_ASSEMBLY_USAGE_OCCURRENCE ( 'NAUO59', ' ', ' ', #6540, #12069, $ ) ;
#13100 = NEXT_ASSEMBLY_USAGE_OCCURRENCE ( 'NAUO60', ' ', ' ', #6540, #12069, $ ) ;
#13101 = NEXT_ASSEMBLY_USAGE_OCCURRENCE ( 'NAUO61', ' ', ' ', #6540, #12069, $ ) ;
#13102 = NEXT_ASSEMBLY_USAGE_OCCURRENCE ( 'NAUO62', ' ', ' ', #6540, #12069, $ ) ;
#13103 = NEXT_ASSEMBLY_USAGE_OCCURRENCE ( 'NAUO63', ' ', ' ', #6540, #12069, $ ) ;
#13104 = NEXT_ASSEMBLY_USAGE_OCCURRENCE ( 'NAUO64', ' ', ' ', #6540, #12069, $ ) ;
#13105 = NEXT_ASSEMBLY_USAGE_OCCURRENCE ( 'NAUO65', ' ', ' ', #6540, #12069, $ ) ;
#13106 = NEXT_ASSEMBLY_USAGE_OCCURRENCE ( 'NAUO66', ' ', ' ', #6540, #12069, $ ) ;
#13107 = NEXT_ASSEMBLY_USAGE_OCCURRENCE ( 'NAUO67', ' ', ' ', #6540, #12069, $ ) ;
#13108 = NEXT_ASSEMBLY_USAGE_OCCURRENCE ( 'NAUO68', ' ', ' ', #6540, #12069, $ ) ;
#13109 = NEXT_ASSEMBLY_USAGE_OCCURRENCE ( 'NAUO69', ' ', ' ', #6540, #12069, $ ) ;
#13110 = NEXT_ASSEMBLY_USAGE_OCCURRENCE ( 'NAUO70', ' ', ' ', #6540, #12069, $ ) ;
#13111 = NEXT_ASSEMBLY_USAGE_OCCURRENCE ( 'NAUO71', ' ', ' ', #6540, #12069, $ ) ;
#13112 = NEXT_ASSEMBLY_USAGE_OCCURRENCE ( 'NAUO72', ' ', ' ', #6540, #12069, $ ) ;
#13113 = NEXT_ASSEMBLY_USAGE_OCCURRENCE ( 'NAUO73', ' ', ' ', #6540, #12069, $ ) ;
#13114 = NEXT_ASSEMBLY_USAGE_OCCURRENCE ( 'NAUO74', ' ', ' ', #6540, #12069, $ ) ;
#13115 = NEXT_ASSEMBLY_USAGE_OCCURRENCE ( 'NAUO75', ' ', ' ', #6540, #12069, $ ) ;
#13116 = NEXT_ASSEMBLY_USAGE_OCCURRENCE ( 'NAUO76', ' ', ' ', #6540, #12069, $ ) ;
#13117 = NEXT_ASSEMBLY_USAGE_OCCURRENCE ( 'NAUO77', ' ', ' ', #6540, #12069, $ ) ;
#13118 = NEXT_ASSEMBLY_USAGE_OCCURRENCE ( 'NAUO78', ' ', ' ', #6540, #12069, $ ) ;
#13119 = NEXT_ASSEMBLY_USAGE_OCCURRENCE ( 'NAUO79', ' ', ' ', #6540, #12069, $ ) ;
#13120 = NEXT_ASSEMBLY_USAGE_OCCURRENCE ( 'NAUO80', ' ', ' ', #6540, #10447, $ ) ;
#13121 = NEXT_ASSEMBLY_USAGE_OCCURRENCE ( 'NAUO81', ' ', ' ', #6540, #10447, $ ) ;
#13122 = NEXT_ASSEMBLY_USAGE_OCCURRENCE ( 'NAUO82', ' ', ' ', #6540, #10447, $ ) ;
#13123 = NEXT_ASSEMBLY_USAGE_OCCURRENCE ( 'NAUO83', ' ', ' ', #6540, #10447, $ ) ;
#13124 = NEXT_ASSEMBLY_USAGE_OCCURRENCE ( 'NAUO84', ' ', ' ', #6540, #10447, $ ) ;
#13125 = NEXT_ASSEMBLY_USAGE_OCCURRENCE ( 'NAUO85', ' ', ' ', #6540, #10447, $ ) ;
#13126 = NEXT_ASSEMBLY_USAGE_OCCURRENCE ( 'NAUO86', ' ', ' ', #6540, #10447, $ ) ;
#13127 = NEXT_ASSEMBLY_USAGE_OCCURRENCE ( 'NAUO87', ' ', ' ', #6540, #10447, $ ) ;
#13128 = NEXT_ASSEMBLY_USAGE_OCCURRENCE ( 'NAUO88', ' ', ' ', #6540, #10447, $ ) ;
#13129 = NEXT_ASSEMBLY_USAGE_OCCURRENCE ( 'NAUO89', ' ', ' ', #6540, #10447, $ ) ;
#13130 = NEXT_ASSEMBLY_USAGE_OCCURRENCE ( 'NAUO90', ' ', ' ', #6540, #10447, $ ) ;
#13131 = NEXT_ASSEMBLY_USAGE_OCCURRENCE ( 'NAUO91', ' ', ' ', #6540, #10447, $ ) ;
#13132 = NEXT_ASSEMBLY_USAGE_OCCURRENCE ( 'NAUO92', ' ', ' ', #6540, #10447, $ ) ;
#13133 = NEXT_ASSEMBLY_USAGE_OCCURRENCE ( 'NAUO93', ' ', ' ', #6540, #10447, $ ) ;
#13134 = NEXT_ASSEMBLY_USAGE_OCCURRENCE ( 'NAUO94', ' ', ' ', #6540, #10447, $ ) ;
#13135 = NEXT_ASSEMBLY_USAGE_OCCURRENCE ( 'NAUO95', ' ', ' ', #6540, #10447, $ ) ;
#13136 = NEXT_ASSEMBLY_USAGE_OCCURRENCE ( 'NAUO96', ' ', ' ', #6540, #10447, $ ) ;
#13137 = NEXT_ASSEMBLY_USAGE_OCCURRENCE ( 'NAUO97', ' ', ' ', #6540, #10447, $ ) ;
#13138 = NEXT_ASSEMBLY_USAGE_OCCURRENCE ( 'NAUO98', ' ', ' ', #6540, #10447, $ ) ;
#13139 = NEXT_ASSEMBLY_USAGE_OCCURRENCE ( 'NAUO99', ' ', ' ', #6540, #10447, $ ) ;
#13140 = NEXT_ASSEMBLY_USAGE_OCCURRENCE ( 'NAUO100', ' ', ' ', #6540, #10447, $ ) ;
#13141 = NEXT_ASSEMBLY_USAGE_OCCURRENCE ( 'NAUO101', ' ', ' ', #6540, #10447, $ ) ;
#13142 = NEXT_ASSEMBLY_USAGE_OCCURRENCE ( 'NAUO102', ' ', ' ', #6540, #10447, $ ) ;
#13143 = NEXT_ASSEMBLY_USAGE_OCCURRENCE ( 'NAUO103', ' ', ' ', #6540, #10447, $ ) ;
#13144 = NEXT_ASSEMBLY_USAGE_OCCURRENCE ( 'NAUO104', ' ', ' ', #6540, #10447, $ ) ;
#13145 = NEXT_ASSEMBLY_USAGE_OCCURRENCE ( 'NAUO105', ' ', ' ', #6540, #10447, $ ) ;
#13146 = NEXT_ASSEMBLY_USAGE_OCCURRENCE ( 'NAUO106', ' ', ' ', #6540, #10447, $ ) ;
#13147 = NEXT_ASSEMBLY_USAGE_OCCURRENCE ( 'NAUO107', ' ', ' ', #6540, #10447, $ ) ;
#13148 = NEXT_ASSEMBLY_USAGE_OCCURRENCE ( 'NAUO108', ' ', ' ', #6540, #10447, $ ) ;
#13149 = NEXT_ASSEMBLY_USAGE_OCCURRENCE ( 'NAUO109', ' ', ' ', #6540, #10447, $ ) ;
#13150 = NEXT_ASSEMBLY_USAGE_OCCURRENCE ( 'NAUO110', ' ', ' ', #6540, #10447, $ ) ;
#13151 = NEXT_ASSEMBLY_USAGE_OCCURRENCE ( 'NAUO111', ' ', ' ', #6540, #10447, $ ) ;
#13152 = NEXT_ASSEMBLY_USAGE_OCCURRENCE ( 'NAUO112', ' ', ' ', #6540, #10447, $ ) ;
#13153 = NEXT_ASSEMBLY_USAGE_OCCURRENCE ( 'NAUO113', ' ', ' ', #6540, #10447, $ ) ;
#13154 = NEXT_ASSEMBLY_USAGE_OCCURRENCE ( 'NAUO114', ' ', ' ', #6540, #10447, $ ) ;
#13155 = NEXT_ASSEMBLY_USAGE_OCCURRENCE ( 'NAUO115', ' ', ' ', #6540, #10447, $ ) ;
#13156 = NEXT_ASSEMBLY_USAGE_OCCURRENCE ( 'NAUO116', ' ', ' ', #6540, #10447, $ ) ;
#13157 = NEXT_ASSEMBLY_USAGE_OCCURRENCE ( 'NAUO117', ' ', ' ', #6540, #10447, $ ) ;
#13158 = NEXT_ASSEMBLY_USAGE_OCCURRENCE ( 'NAUO118', ' ', ' ', #6540, #10447, $ ) ;
#13159 = NEXT_ASSEMBLY_USAGE_OCCURRENCE ( 'NAUO119', ' ', ' ', #6540, #10447, $ ) ;
#13160 = NEXT_ASSEMBLY_USAGE_OCCURRENCE ( 'NAUO120', ' ', ' ', #6540, #10447, $ ) ;
#13161 = NEXT_ASSEMBLY_USAGE_OCCURRENCE ( 'NAUO121', ' ', ' ', #6540, #10447, $ ) ;
#13162 = NEXT_ASSEMBLY_USAGE_OCCURRENCE ( 'NAUO122', ' ', ' ', #6540, #10447, $ ) ;
#13163 = NEXT_ASSEMBLY_USAGE_OCCURRENCE ( 'NAUO123', ' ', ' ', #6540, #10447, $ ) ;
#13164 = NEXT_ASSEMBLY_USAGE_OCCURRENCE ( 'NAUO124', ' ', ' ', #6540, #10447, $ ) ;
#13165 = NEXT_ASSEMBLY_USAGE_OCCURRENCE ( 'NAUO125', ' ', ' ', #6540, #10447, $ ) ;
#13166 = NEXT_ASSEMBLY_USAGE_OCCURRENCE ( 'NAUO126', ' ', ' ', #6540, #10447, $ ) ;
#13167 = NEXT_ASSEMBLY_USAGE_OCCURRENCE ( 'NAUO127', ' ', ' ', #6540, #10447, $ ) ;
#13168 = NEXT_ASSEMBLY_USAGE_OCCURRENCE ( 'NAUO128', ' ', ' ', #6540, #10447, $ ) ;
#13169 = NEXT_ASSEMBLY_USAGE_OCCURRENCE ( 'NAUO129', ' ', ' ', #6540, #10447, $ ) ;
#13170 = NEXT_ASSEMBLY_USAGE_OCCURRENCE ( 'NAUO130', ' ', ' ', #6540, #10447, $ ) ;
#13171 = NEXT_ASSEMBLY_USAGE_OCCURRENCE ( 'NAUO131', ' ', ' ', #6540, #10447, $ ) ;
#13172 = NEXT_ASSEMBLY_USAGE_OCCURRENCE ( 'NAUO132', ' ', ' ', #6540, #10447, $ ) ;
#13173 = NEXT_ASSEMBLY_USAGE_OCCURRENCE ( 'NAUO133', ' ', ' ', #6540, #10447, $ ) ;
#13174 = NEXT_ASSEMBLY_USAGE_OCCURRENCE ( 'NAUO134', ' ', ' ', #6540, #10447, $ ) ;
#13175 = NEXT_ASSEMBLY_USAGE_OCCURRENCE ( 'NAUO135', ' ', ' ', #6540, #10447, $ ) ;
#13176 = NEXT_ASSEMBLY_USAGE_OCCURRENCE ( 'NAUO136', ' ', ' ', #6540, #10447, $ ) ;
#13177 = NEXT_ASSEMBLY_USAGE_OCCURRENCE ( 'NAUO137', ' ', ' ', #6540, #10447, $ ) ;
#13178 = NEXT_ASSEMBLY_USAGE_OCCURRENCE ( 'NAUO138', ' ', ' ', #6540, #10447, $ ) ;
#13179 = NEXT_ASSEMBLY_USAGE_OCCURRENCE ( 'NAUO139', ' ', ' ', #6540, #10447, $ ) ;
#13180 = NEXT_ASSEMBLY_USAGE_OCCURRENCE ( 'NAUO140', ' ', ' ', #6540, #10447, $ ) ;
#13181 = NEXT_ASSEMBLY_USAGE_OCCURRENCE ( 'NAUO141', ' ', ' ', #6540, #10447, $ ) ;
#13182 = NEXT_ASSEMBLY_USAGE_OCCURRENCE ( 'NAUO142', ' ', ' ', #6540, #10447, $ ) ;
#13183 = NEXT_ASSEMBLY_USAGE_OCCURRENCE ( 'NAUO143', ' ', ' ', #6540, #10447, $ ) ;
#13184 = NEXT_ASSEMBLY_USAGE_OCCURRENCE ( 'NAUO144', ' ', ' ', #6540, #10447, $ ) ;
#13185 = NEXT_ASSEMBLY_USAGE_OCCURRENCE ( 'NAUO145', ' ', ' ', #6540, #10447, $ ) ;
#13186 = NEXT_ASSEMBLY_USAGE_OCCURRENCE ( 'NAUO146', ' ', ' ', #6540, #10447, $ ) ;
#13187 = NEXT_ASSEMBLY_USAGE_OCCURRENCE ( 'NAUO147', ' ', ' ', #6540, #10447, $ ) ;
#13188 = NEXT_ASSEMBLY_USAGE_OCCURRENCE ( 'NAUO148', ' ', ' ', #6540, #10447, $ ) ;
#13189 = NEXT_ASSEMBLY_USAGE_OCCURRENCE ( 'NAUO149', ' ', ' ', #6540, #10447, $ ) ;
#13190 = NEXT_ASSEMBLY_USAGE_OCCURRENCE ( 'NAUO150', ' ', ' ', #6540, #10447, $ ) ;
ENDSEC;
END-ISO-10303-21;
